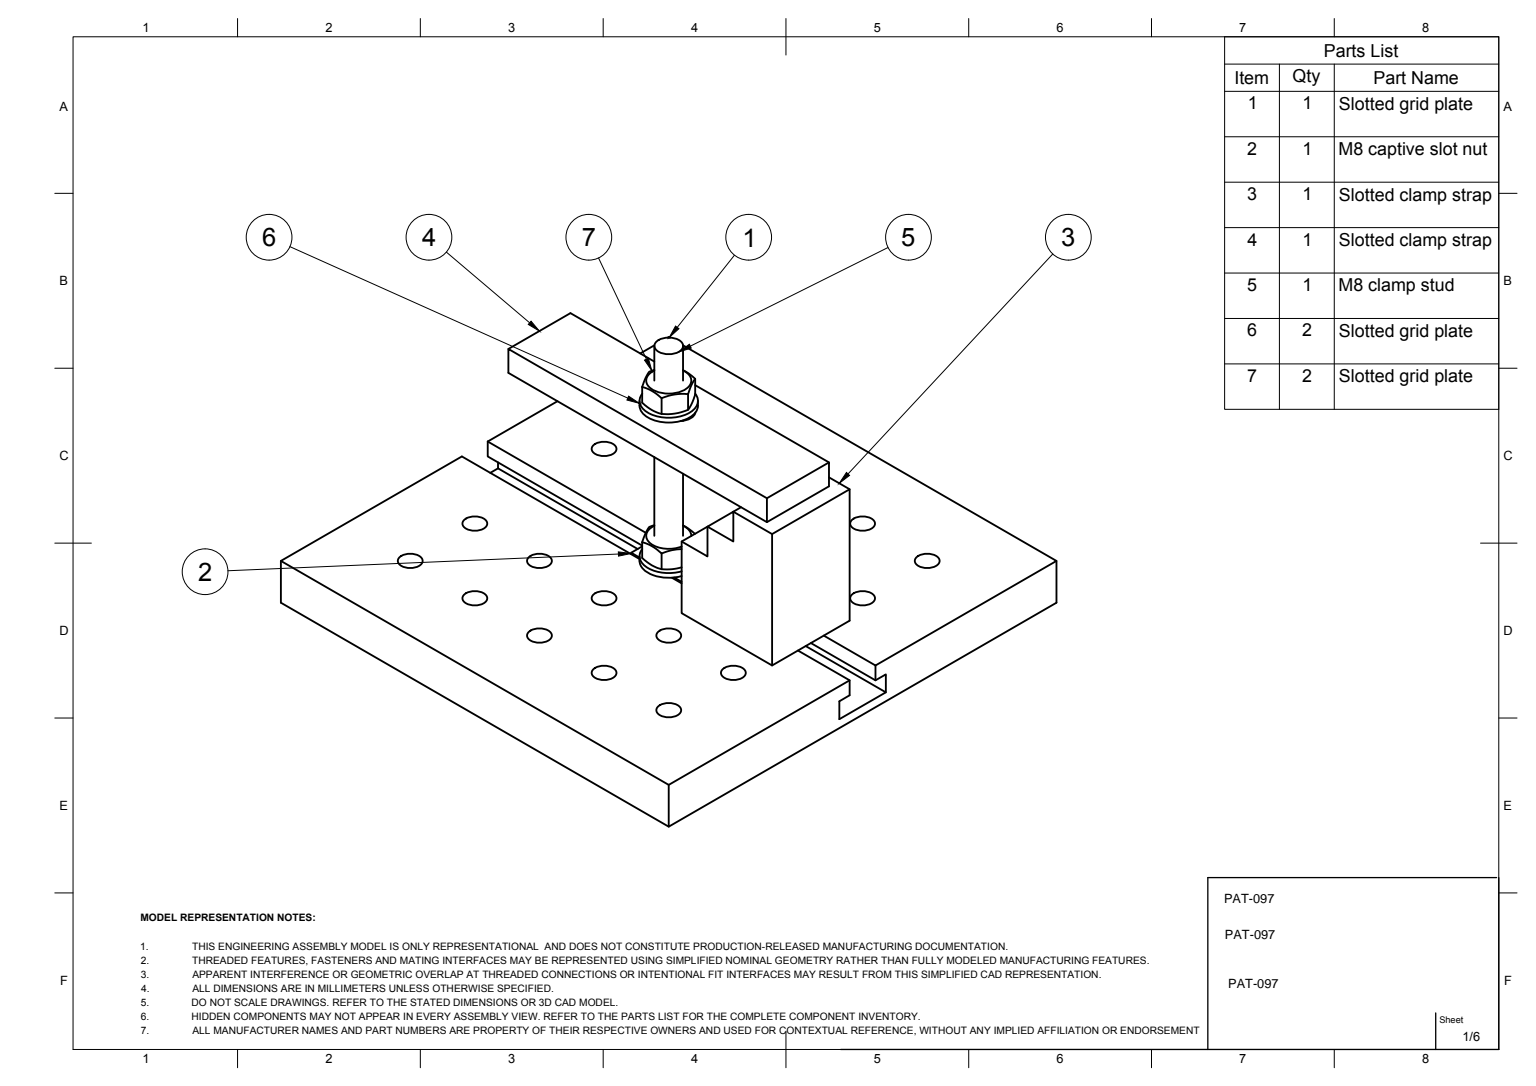
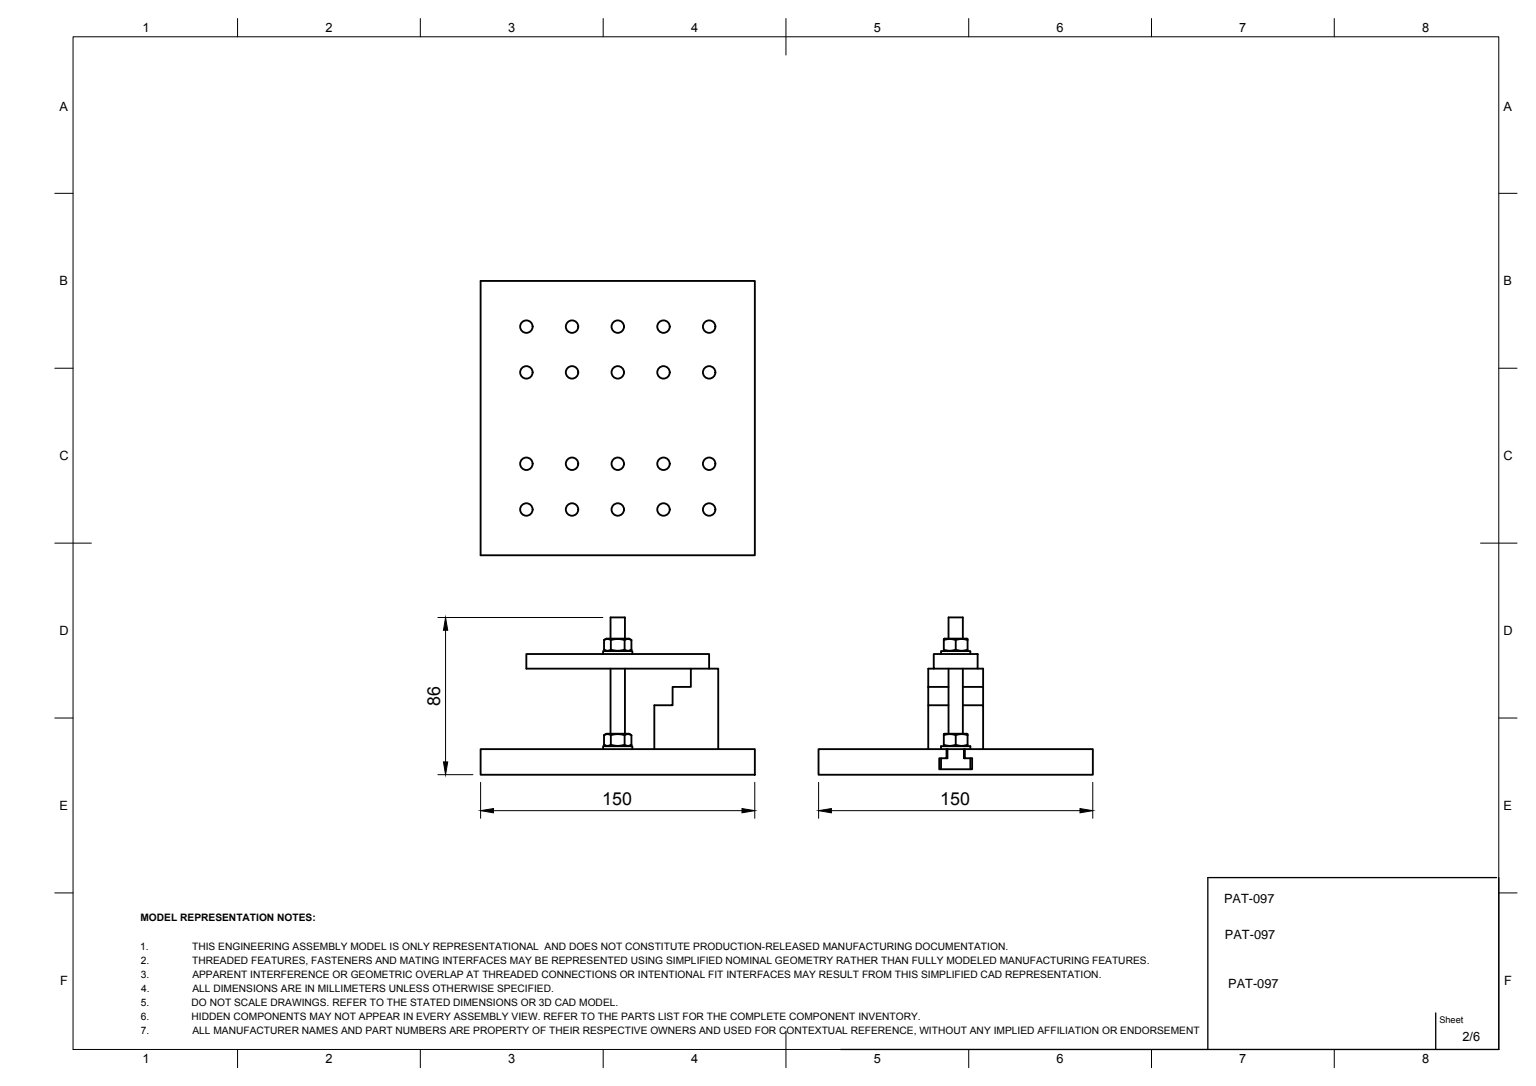
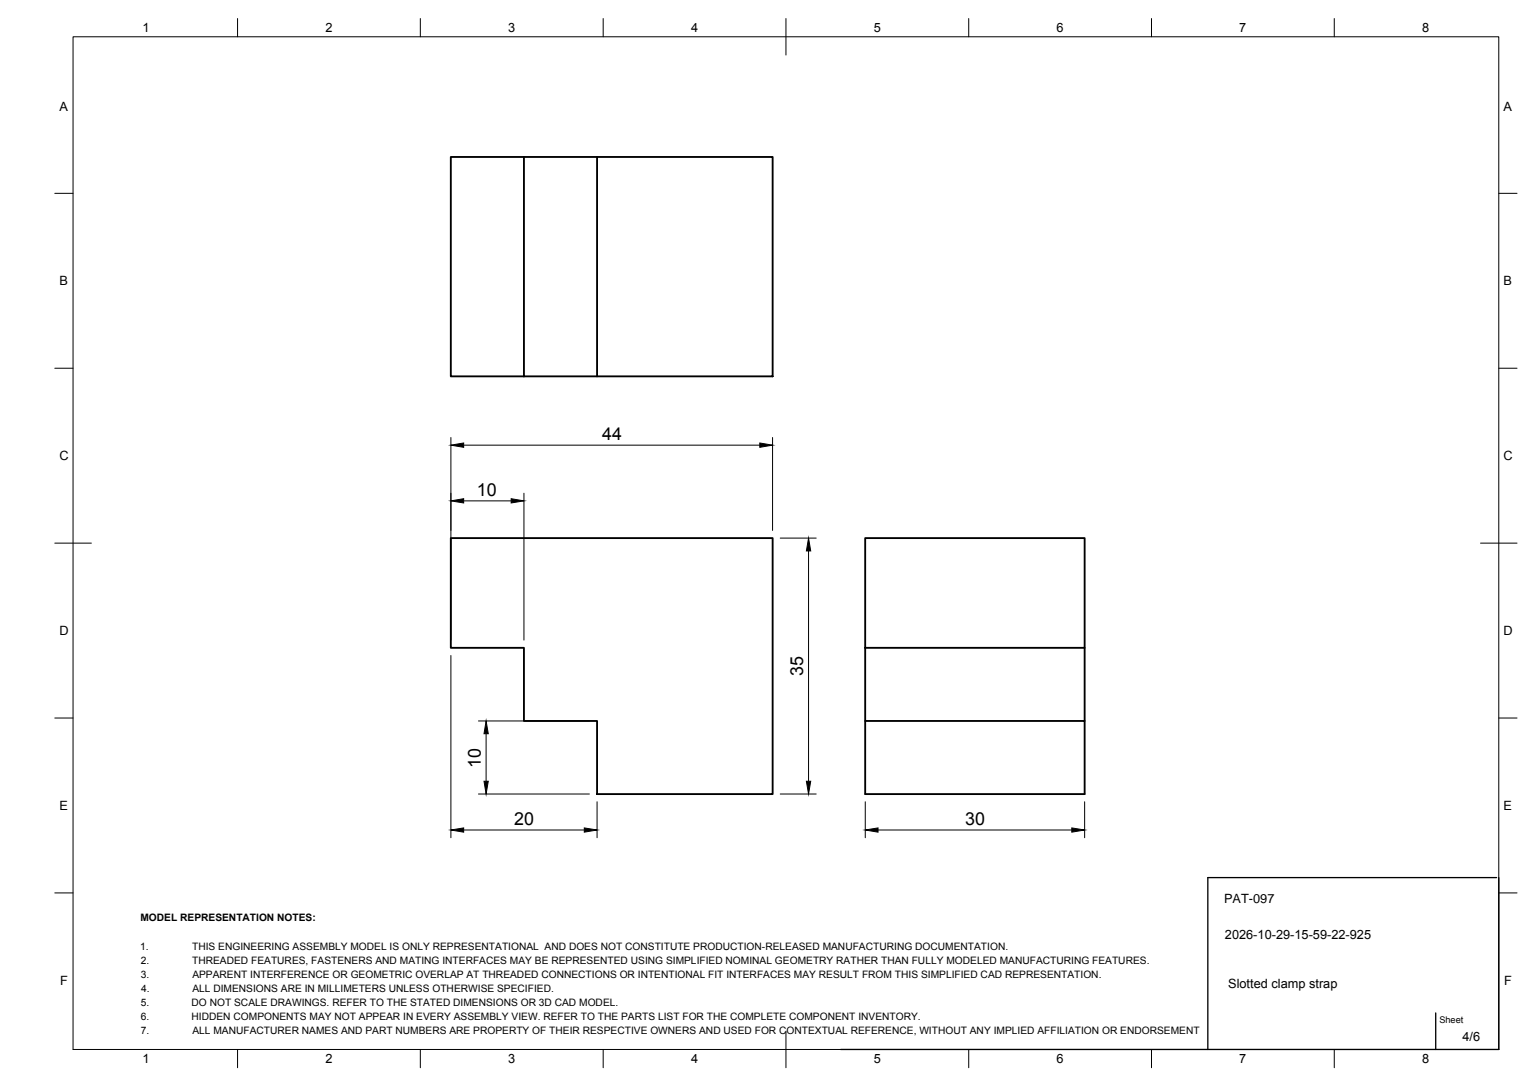
ISO-10303-21;
HEADER;
/* Generated by software containing ST-Developer
 * from STEP Tools, Inc. (www.steptools.com) 
 */

FILE_DESCRIPTION(
/* description */ ('PAT-097'),
/* implementation_level */ '2;1');

FILE_NAME(
/* name */ 'PAT-097',
/* time_stamp */ '2026-10-29T15:59:31-07:00',
/* author */ (''),
/* organization */ (''),
/* preprocessor_version */ 'ST-DEVELOPER v20.2',
/* originating_system */ 'Autodesk Translation Framework v15.17.0.0',
/* authorisation */ '');

FILE_SCHEMA (('AUTOMOTIVE_DESIGN { 1 0 10303 214 3 1 1 }'));
ENDSEC;

DATA;
#10=MECHANICAL_DESIGN_GEOMETRIC_PRESENTATION_REPRESENTATION('',(#75,#76,
#77,#78,#79,#80,#81),#2768);
#11=ITEM_DEFINED_TRANSFORMATION($,$,#1682,#1828);
#12=ITEM_DEFINED_TRANSFORMATION($,$,#1757,#1829);
#13=ITEM_DEFINED_TRANSFORMATION($,$,#1771,#1830);
#14=ITEM_DEFINED_TRANSFORMATION($,$,#1782,#1831);
#15=ITEM_DEFINED_TRANSFORMATION($,$,#1797,#1832);
#16=ITEM_DEFINED_TRANSFORMATION($,$,#1803,#1833);
#17=ITEM_DEFINED_TRANSFORMATION($,$,#1812,#1834);
#18=ITEM_DEFINED_TRANSFORMATION($,$,#1803,#1835);
#19=ITEM_DEFINED_TRANSFORMATION($,$,#1812,#1836);
#20=(
REPRESENTATION_RELATIONSHIP($,$,#2799,#2798)
REPRESENTATION_RELATIONSHIP_WITH_TRANSFORMATION(#11)
SHAPE_REPRESENTATION_RELATIONSHIP()
);
#21=(
REPRESENTATION_RELATIONSHIP($,$,#2800,#2798)
REPRESENTATION_RELATIONSHIP_WITH_TRANSFORMATION(#12)
SHAPE_REPRESENTATION_RELATIONSHIP()
);
#22=(
REPRESENTATION_RELATIONSHIP($,$,#2801,#2798)
REPRESENTATION_RELATIONSHIP_WITH_TRANSFORMATION(#13)
SHAPE_REPRESENTATION_RELATIONSHIP()
);
#23=(
REPRESENTATION_RELATIONSHIP($,$,#2802,#2798)
REPRESENTATION_RELATIONSHIP_WITH_TRANSFORMATION(#14)
SHAPE_REPRESENTATION_RELATIONSHIP()
);
#24=(
REPRESENTATION_RELATIONSHIP($,$,#2803,#2798)
REPRESENTATION_RELATIONSHIP_WITH_TRANSFORMATION(#15)
SHAPE_REPRESENTATION_RELATIONSHIP()
);
#25=(
REPRESENTATION_RELATIONSHIP($,$,#2804,#2798)
REPRESENTATION_RELATIONSHIP_WITH_TRANSFORMATION(#16)
SHAPE_REPRESENTATION_RELATIONSHIP()
);
#26=(
REPRESENTATION_RELATIONSHIP($,$,#2805,#2798)
REPRESENTATION_RELATIONSHIP_WITH_TRANSFORMATION(#17)
SHAPE_REPRESENTATION_RELATIONSHIP()
);
#27=(
REPRESENTATION_RELATIONSHIP($,$,#2804,#2798)
REPRESENTATION_RELATIONSHIP_WITH_TRANSFORMATION(#18)
SHAPE_REPRESENTATION_RELATIONSHIP()
);
#28=(
REPRESENTATION_RELATIONSHIP($,$,#2805,#2798)
REPRESENTATION_RELATIONSHIP_WITH_TRANSFORMATION(#19)
SHAPE_REPRESENTATION_RELATIONSHIP()
);
#29=CONTEXT_DEPENDENT_SHAPE_REPRESENTATION(#20,#2789);
#30=CONTEXT_DEPENDENT_SHAPE_REPRESENTATION(#21,#2790);
#31=CONTEXT_DEPENDENT_SHAPE_REPRESENTATION(#22,#2791);
#32=CONTEXT_DEPENDENT_SHAPE_REPRESENTATION(#23,#2792);
#33=CONTEXT_DEPENDENT_SHAPE_REPRESENTATION(#24,#2793);
#34=CONTEXT_DEPENDENT_SHAPE_REPRESENTATION(#25,#2794);
#35=CONTEXT_DEPENDENT_SHAPE_REPRESENTATION(#26,#2795);
#36=CONTEXT_DEPENDENT_SHAPE_REPRESENTATION(#27,#2796);
#37=CONTEXT_DEPENDENT_SHAPE_REPRESENTATION(#28,#2797);
#38=NEXT_ASSEMBLY_USAGE_OCCURRENCE('Slotted grid plate:1',
'Slotted grid plate:1','Slotted grid plate:1',#2807,#2808,
'Slotted grid plate:1');
#39=NEXT_ASSEMBLY_USAGE_OCCURRENCE('M8 captive slot nut:1',
'M8 captive slot nut:1','M8 captive slot nut:1',#2807,#2809,
'M8 captive slot nut:1');
#40=NEXT_ASSEMBLY_USAGE_OCCURRENCE('Stepped heel block:1',
'Stepped heel block:1','Stepped heel block:1',#2807,#2810,
'Stepped heel block:1');
#41=NEXT_ASSEMBLY_USAGE_OCCURRENCE('Slotted clamp strap:1',
'Slotted clamp strap:1','Slotted clamp strap:1',#2807,#2811,
'Slotted clamp strap:1');
#42=NEXT_ASSEMBLY_USAGE_OCCURRENCE('M8 clamp stud:1','M8 clamp stud:1',
'M8 clamp stud:1',#2807,#2812,'M8 clamp stud:1');
#43=NEXT_ASSEMBLY_USAGE_OCCURRENCE('Flat Washer - M8:1',
'Flat Washer - M8:1','Flat Washer - M8:1',#2807,#2813,
'Flat Washer - M8:1');
#44=NEXT_ASSEMBLY_USAGE_OCCURRENCE('Hex Nut - M8:1','Hex Nut - M8:1',
'Hex Nut - M8:1',#2807,#2814,'Hex Nut - M8:1');
#45=NEXT_ASSEMBLY_USAGE_OCCURRENCE('Flat Washer - M8:2',
'Flat Washer - M8:2','Flat Washer - M8:2',#2807,#2813,
'Flat Washer - M8:2');
#46=NEXT_ASSEMBLY_USAGE_OCCURRENCE('Hex Nut - M8:2','Hex Nut - M8:2',
'Hex Nut - M8:2',#2807,#2814,'Hex Nut - M8:2');
#47=(
BOUNDED_CURVE()
B_SPLINE_CURVE(2,(#2669,#2670,#2671),.UNSPECIFIED.,.F.,.F.)
B_SPLINE_CURVE_WITH_KNOTS((3,3),(0.14973948338295,0.97160236658079),
 .UNSPECIFIED.)
CURVE()
GEOMETRIC_REPRESENTATION_ITEM()
RATIONAL_B_SPLINE_CURVE((1.07140024848292,1.23714644374248,1.07140024848292))
REPRESENTATION_ITEM('')
);
#48=(
BOUNDED_CURVE()
B_SPLINE_CURVE(2,(#2673,#2674,#2675),.UNSPECIFIED.,.F.,.F.)
B_SPLINE_CURVE_WITH_KNOTS((3,3),(0.14973948338295,0.971602366580789),
 .UNSPECIFIED.)
CURVE()
GEOMETRIC_REPRESENTATION_ITEM()
RATIONAL_B_SPLINE_CURVE((1.07140024848292,1.23714644374248,1.07140024848292))
REPRESENTATION_ITEM('')
);
#49=(
BOUNDED_CURVE()
B_SPLINE_CURVE(2,(#2680,#2681,#2682),.UNSPECIFIED.,.F.,.F.)
B_SPLINE_CURVE_WITH_KNOTS((3,3),(0.14973948338295,0.97160236658079),
 .UNSPECIFIED.)
CURVE()
GEOMETRIC_REPRESENTATION_ITEM()
RATIONAL_B_SPLINE_CURVE((1.07140024848292,1.23714644374248,1.07140024848292))
REPRESENTATION_ITEM('')
);
#50=(
BOUNDED_CURVE()
B_SPLINE_CURVE(2,(#2684,#2685,#2686),.UNSPECIFIED.,.F.,.F.)
B_SPLINE_CURVE_WITH_KNOTS((3,3),(0.14973948338295,0.97160236658079),
 .UNSPECIFIED.)
CURVE()
GEOMETRIC_REPRESENTATION_ITEM()
RATIONAL_B_SPLINE_CURVE((1.07140024848292,1.23714644374248,1.07140024848292))
REPRESENTATION_ITEM('')
);
#51=(
BOUNDED_CURVE()
B_SPLINE_CURVE(2,(#2688,#2689,#2690),.UNSPECIFIED.,.F.,.F.)
B_SPLINE_CURVE_WITH_KNOTS((3,3),(0.14973948338295,0.971602366580789),
 .UNSPECIFIED.)
CURVE()
GEOMETRIC_REPRESENTATION_ITEM()
RATIONAL_B_SPLINE_CURVE((1.07140024848292,1.23714644374248,1.07140024848292))
REPRESENTATION_ITEM('')
);
#52=(
BOUNDED_CURVE()
B_SPLINE_CURVE(2,(#2691,#2692,#2693),.UNSPECIFIED.,.F.,.F.)
B_SPLINE_CURVE_WITH_KNOTS((3,3),(0.14973948338295,0.97160236658079),
 .UNSPECIFIED.)
CURVE()
GEOMETRIC_REPRESENTATION_ITEM()
RATIONAL_B_SPLINE_CURVE((1.07140024848292,1.23714644374248,1.07140024848292))
REPRESENTATION_ITEM('')
);
#53=(
BOUNDED_CURVE()
B_SPLINE_CURVE(2,(#2700,#2701,#2702),.UNSPECIFIED.,.F.,.F.)
B_SPLINE_CURVE_WITH_KNOTS((3,3),(0.14973948338295,0.97160236658079),
 .UNSPECIFIED.)
CURVE()
GEOMETRIC_REPRESENTATION_ITEM()
RATIONAL_B_SPLINE_CURVE((1.07140024848292,1.23714644374248,1.07140024848292))
REPRESENTATION_ITEM('')
);
#54=(
BOUNDED_CURVE()
B_SPLINE_CURVE(2,(#2704,#2705,#2706),.UNSPECIFIED.,.F.,.F.)
B_SPLINE_CURVE_WITH_KNOTS((3,3),(0.14973948338295,0.97160236658079),
 .UNSPECIFIED.)
CURVE()
GEOMETRIC_REPRESENTATION_ITEM()
RATIONAL_B_SPLINE_CURVE((1.07140024848292,1.23714644374248,1.07140024848292))
REPRESENTATION_ITEM('')
);
#55=(
BOUNDED_CURVE()
B_SPLINE_CURVE(2,(#2708,#2709,#2710),.UNSPECIFIED.,.F.,.F.)
B_SPLINE_CURVE_WITH_KNOTS((3,3),(0.14973948338295,0.971602366580789),
 .UNSPECIFIED.)
CURVE()
GEOMETRIC_REPRESENTATION_ITEM()
RATIONAL_B_SPLINE_CURVE((1.07140024848292,1.23714644374248,1.07140024848292))
REPRESENTATION_ITEM('')
);
#56=(
BOUNDED_CURVE()
B_SPLINE_CURVE(2,(#2712,#2713,#2714),.UNSPECIFIED.,.F.,.F.)
B_SPLINE_CURVE_WITH_KNOTS((3,3),(0.14973948338295,0.97160236658079),
 .UNSPECIFIED.)
CURVE()
GEOMETRIC_REPRESENTATION_ITEM()
RATIONAL_B_SPLINE_CURVE((1.07140024848292,1.23714644374248,1.07140024848292))
REPRESENTATION_ITEM('')
);
#57=(
BOUNDED_CURVE()
B_SPLINE_CURVE(2,(#2716,#2717,#2718),.UNSPECIFIED.,.F.,.F.)
B_SPLINE_CURVE_WITH_KNOTS((3,3),(0.14973948338295,0.97160236658079),
 .UNSPECIFIED.)
CURVE()
GEOMETRIC_REPRESENTATION_ITEM()
RATIONAL_B_SPLINE_CURVE((1.07140024848292,1.23714644374248,1.07140024848292))
REPRESENTATION_ITEM('')
);
#58=(
BOUNDED_CURVE()
B_SPLINE_CURVE(2,(#2719,#2720,#2721),.UNSPECIFIED.,.F.,.F.)
B_SPLINE_CURVE_WITH_KNOTS((3,3),(0.14973948338295,0.971602366580789),
 .UNSPECIFIED.)
CURVE()
GEOMETRIC_REPRESENTATION_ITEM()
RATIONAL_B_SPLINE_CURVE((1.07140024848292,1.23714644374248,1.07140024848292))
REPRESENTATION_ITEM('')
);
#59=CONICAL_SURFACE('',#1813,0.734027674973257,1.0471975511966);
#60=CONICAL_SURFACE('',#1815,0.734027674973257,1.0471975511966);
#61=SHAPE_REPRESENTATION_RELATIONSHIP('SRR','None',#2799,#68);
#62=SHAPE_REPRESENTATION_RELATIONSHIP('SRR','None',#2800,#69);
#63=SHAPE_REPRESENTATION_RELATIONSHIP('SRR','None',#2801,#70);
#64=SHAPE_REPRESENTATION_RELATIONSHIP('SRR','None',#2802,#71);
#65=SHAPE_REPRESENTATION_RELATIONSHIP('SRR','None',#2803,#72);
#66=SHAPE_REPRESENTATION_RELATIONSHIP('SRR','None',#2804,#73);
#67=SHAPE_REPRESENTATION_RELATIONSHIP('SRR','None',#2805,#74);
#68=ADVANCED_BREP_SHAPE_REPRESENTATION('',(#82),#2761);
#69=ADVANCED_BREP_SHAPE_REPRESENTATION('',(#83),#2762);
#70=ADVANCED_BREP_SHAPE_REPRESENTATION('',(#84),#2763);
#71=ADVANCED_BREP_SHAPE_REPRESENTATION('',(#85),#2764);
#72=ADVANCED_BREP_SHAPE_REPRESENTATION('',(#86),#2765);
#73=ADVANCED_BREP_SHAPE_REPRESENTATION('',(#87),#2766);
#74=ADVANCED_BREP_SHAPE_REPRESENTATION('',(#88),#2767);
#75=STYLED_ITEM('',(#2925),#82);
#76=STYLED_ITEM('',(#2918),#83);
#77=STYLED_ITEM('',(#2890),#84);
#78=STYLED_ITEM('',(#2925),#85);
#79=STYLED_ITEM('',(#2918),#86);
#80=STYLED_ITEM('',(#2918),#87);
#81=STYLED_ITEM('',(#2918),#88);
#82=MANIFOLD_SOLID_BREP('Body1',#1596);
#83=MANIFOLD_SOLID_BREP('Body1',#1597);
#84=MANIFOLD_SOLID_BREP('Body1',#1598);
#85=MANIFOLD_SOLID_BREP('Body1',#1599);
#86=MANIFOLD_SOLID_BREP('Body1',#1600);
#87=MANIFOLD_SOLID_BREP('Body1',#1601);
#88=MANIFOLD_SOLID_BREP('Body1',#1602);
#89=CYLINDRICAL_SURFACE('',#1713,0.34);
#90=CYLINDRICAL_SURFACE('',#1715,0.34);
#91=CYLINDRICAL_SURFACE('',#1717,0.34);
#92=CYLINDRICAL_SURFACE('',#1719,0.34);
#93=CYLINDRICAL_SURFACE('',#1721,0.34);
#94=CYLINDRICAL_SURFACE('',#1723,0.34);
#95=CYLINDRICAL_SURFACE('',#1725,0.34);
#96=CYLINDRICAL_SURFACE('',#1727,0.34);
#97=CYLINDRICAL_SURFACE('',#1729,0.34);
#98=CYLINDRICAL_SURFACE('',#1731,0.34);
#99=CYLINDRICAL_SURFACE('',#1733,0.34);
#100=CYLINDRICAL_SURFACE('',#1735,0.34);
#101=CYLINDRICAL_SURFACE('',#1737,0.34);
#102=CYLINDRICAL_SURFACE('',#1739,0.34);
#103=CYLINDRICAL_SURFACE('',#1741,0.34);
#104=CYLINDRICAL_SURFACE('',#1743,0.34);
#105=CYLINDRICAL_SURFACE('',#1745,0.34);
#106=CYLINDRICAL_SURFACE('',#1747,0.34);
#107=CYLINDRICAL_SURFACE('',#1749,0.34);
#108=CYLINDRICAL_SURFACE('',#1751,0.34);
#109=CYLINDRICAL_SURFACE('',#1758,0.34);
#110=CYLINDRICAL_SURFACE('',#1788,0.45);
#111=CYLINDRICAL_SURFACE('',#1790,0.45);
#112=CYLINDRICAL_SURFACE('',#1798,0.3933);
#113=CYLINDRICAL_SURFACE('',#1804,0.42);
#114=CYLINDRICAL_SURFACE('',#1807,0.8);
#115=CYLINDRICAL_SURFACE('',#1820,0.338975);
#116=FACE_BOUND('',#312,.T.);
#117=FACE_BOUND('',#313,.T.);
#118=FACE_BOUND('',#314,.T.);
#119=FACE_BOUND('',#315,.T.);
#120=FACE_BOUND('',#316,.T.);
#121=FACE_BOUND('',#317,.T.);
#122=FACE_BOUND('',#318,.T.);
#123=FACE_BOUND('',#319,.T.);
#124=FACE_BOUND('',#320,.T.);
#125=FACE_BOUND('',#321,.T.);
#126=FACE_BOUND('',#323,.T.);
#127=FACE_BOUND('',#324,.T.);
#128=FACE_BOUND('',#325,.T.);
#129=FACE_BOUND('',#326,.T.);
#130=FACE_BOUND('',#327,.T.);
#131=FACE_BOUND('',#328,.T.);
#132=FACE_BOUND('',#329,.T.);
#133=FACE_BOUND('',#330,.T.);
#134=FACE_BOUND('',#331,.T.);
#135=FACE_BOUND('',#332,.T.);
#136=FACE_BOUND('',#357,.T.);
#137=FACE_BOUND('',#358,.T.);
#138=FACE_BOUND('',#359,.T.);
#139=FACE_BOUND('',#360,.T.);
#140=FACE_BOUND('',#361,.T.);
#141=FACE_BOUND('',#362,.T.);
#142=FACE_BOUND('',#363,.T.);
#143=FACE_BOUND('',#364,.T.);
#144=FACE_BOUND('',#365,.T.);
#145=FACE_BOUND('',#366,.T.);
#146=FACE_BOUND('',#367,.T.);
#147=FACE_BOUND('',#368,.T.);
#148=FACE_BOUND('',#369,.T.);
#149=FACE_BOUND('',#370,.T.);
#150=FACE_BOUND('',#371,.T.);
#151=FACE_BOUND('',#372,.T.);
#152=FACE_BOUND('',#373,.T.);
#153=FACE_BOUND('',#374,.T.);
#154=FACE_BOUND('',#375,.T.);
#155=FACE_BOUND('',#376,.T.);
#156=FACE_BOUND('',#381,.T.);
#157=FACE_BOUND('',#389,.T.);
#158=FACE_BOUND('',#403,.T.);
#159=FACE_BOUND('',#411,.T.);
#160=FACE_BOUND('',#418,.T.);
#161=FACE_BOUND('',#420,.T.);
#162=FACE_BOUND('',#431,.T.);
#163=FACE_BOUND('',#433,.T.);
#164=CIRCLE('',#1692,0.34);
#165=CIRCLE('',#1693,0.34);
#166=CIRCLE('',#1694,0.34);
#167=CIRCLE('',#1695,0.34);
#168=CIRCLE('',#1696,0.34);
#169=CIRCLE('',#1697,0.34);
#170=CIRCLE('',#1698,0.34);
#171=CIRCLE('',#1699,0.34);
#172=CIRCLE('',#1700,0.34);
#173=CIRCLE('',#1701,0.34);
#174=CIRCLE('',#1703,0.34);
#175=CIRCLE('',#1704,0.34);
#176=CIRCLE('',#1705,0.34);
#177=CIRCLE('',#1706,0.34);
#178=CIRCLE('',#1707,0.34);
#179=CIRCLE('',#1708,0.34);
#180=CIRCLE('',#1709,0.34);
#181=CIRCLE('',#1710,0.34);
#182=CIRCLE('',#1711,0.34);
#183=CIRCLE('',#1712,0.34);
#184=CIRCLE('',#1714,0.34);
#185=CIRCLE('',#1716,0.34);
#186=CIRCLE('',#1718,0.34);
#187=CIRCLE('',#1720,0.34);
#188=CIRCLE('',#1722,0.34);
#189=CIRCLE('',#1724,0.34);
#190=CIRCLE('',#1726,0.34);
#191=CIRCLE('',#1728,0.34);
#192=CIRCLE('',#1730,0.34);
#193=CIRCLE('',#1732,0.34);
#194=CIRCLE('',#1734,0.34);
#195=CIRCLE('',#1736,0.34);
#196=CIRCLE('',#1738,0.34);
#197=CIRCLE('',#1740,0.34);
#198=CIRCLE('',#1742,0.34);
#199=CIRCLE('',#1744,0.34);
#200=CIRCLE('',#1746,0.34);
#201=CIRCLE('',#1748,0.34);
#202=CIRCLE('',#1750,0.34);
#203=CIRCLE('',#1752,0.34);
#204=CIRCLE('',#1759,0.34);
#205=CIRCLE('',#1760,0.34);
#206=CIRCLE('',#1786,0.45);
#207=CIRCLE('',#1787,0.45);
#208=CIRCLE('',#1789,0.45);
#209=CIRCLE('',#1791,0.45);
#210=CIRCLE('',#1799,0.3933);
#211=CIRCLE('',#1800,0.3933);
#212=CIRCLE('',#1805,0.42);
#213=CIRCLE('',#1806,0.42);
#214=CIRCLE('',#1808,0.8);
#215=CIRCLE('',#1809,0.8);
#216=CIRCLE('',#1814,0.6175);
#217=CIRCLE('',#1816,0.6175);
#218=CIRCLE('',#1821,0.338975);
#219=CIRCLE('',#1822,0.338975);
#220=FACE_OUTER_BOUND('',#303,.T.);
#221=FACE_OUTER_BOUND('',#304,.T.);
#222=FACE_OUTER_BOUND('',#305,.T.);
#223=FACE_OUTER_BOUND('',#306,.T.);
#224=FACE_OUTER_BOUND('',#307,.T.);
#225=FACE_OUTER_BOUND('',#308,.T.);
#226=FACE_OUTER_BOUND('',#309,.T.);
#227=FACE_OUTER_BOUND('',#310,.T.);
#228=FACE_OUTER_BOUND('',#311,.T.);
#229=FACE_OUTER_BOUND('',#322,.T.);
#230=FACE_OUTER_BOUND('',#333,.T.);
#231=FACE_OUTER_BOUND('',#334,.T.);
#232=FACE_OUTER_BOUND('',#335,.T.);
#233=FACE_OUTER_BOUND('',#336,.T.);
#234=FACE_OUTER_BOUND('',#337,.T.);
#235=FACE_OUTER_BOUND('',#338,.T.);
#236=FACE_OUTER_BOUND('',#339,.T.);
#237=FACE_OUTER_BOUND('',#340,.T.);
#238=FACE_OUTER_BOUND('',#341,.T.);
#239=FACE_OUTER_BOUND('',#342,.T.);
#240=FACE_OUTER_BOUND('',#343,.T.);
#241=FACE_OUTER_BOUND('',#344,.T.);
#242=FACE_OUTER_BOUND('',#345,.T.);
#243=FACE_OUTER_BOUND('',#346,.T.);
#244=FACE_OUTER_BOUND('',#347,.T.);
#245=FACE_OUTER_BOUND('',#348,.T.);
#246=FACE_OUTER_BOUND('',#349,.T.);
#247=FACE_OUTER_BOUND('',#350,.T.);
#248=FACE_OUTER_BOUND('',#351,.T.);
#249=FACE_OUTER_BOUND('',#352,.T.);
#250=FACE_OUTER_BOUND('',#353,.T.);
#251=FACE_OUTER_BOUND('',#354,.T.);
#252=FACE_OUTER_BOUND('',#355,.T.);
#253=FACE_OUTER_BOUND('',#356,.T.);
#254=FACE_OUTER_BOUND('',#377,.T.);
#255=FACE_OUTER_BOUND('',#378,.T.);
#256=FACE_OUTER_BOUND('',#379,.T.);
#257=FACE_OUTER_BOUND('',#380,.T.);
#258=FACE_OUTER_BOUND('',#382,.T.);
#259=FACE_OUTER_BOUND('',#383,.T.);
#260=FACE_OUTER_BOUND('',#384,.T.);
#261=FACE_OUTER_BOUND('',#385,.T.);
#262=FACE_OUTER_BOUND('',#386,.T.);
#263=FACE_OUTER_BOUND('',#387,.T.);
#264=FACE_OUTER_BOUND('',#388,.T.);
#265=FACE_OUTER_BOUND('',#390,.T.);
#266=FACE_OUTER_BOUND('',#391,.T.);
#267=FACE_OUTER_BOUND('',#392,.T.);
#268=FACE_OUTER_BOUND('',#393,.T.);
#269=FACE_OUTER_BOUND('',#394,.T.);
#270=FACE_OUTER_BOUND('',#395,.T.);
#271=FACE_OUTER_BOUND('',#396,.T.);
#272=FACE_OUTER_BOUND('',#397,.T.);
#273=FACE_OUTER_BOUND('',#398,.T.);
#274=FACE_OUTER_BOUND('',#399,.T.);
#275=FACE_OUTER_BOUND('',#400,.T.);
#276=FACE_OUTER_BOUND('',#401,.T.);
#277=FACE_OUTER_BOUND('',#402,.T.);
#278=FACE_OUTER_BOUND('',#404,.T.);
#279=FACE_OUTER_BOUND('',#405,.T.);
#280=FACE_OUTER_BOUND('',#406,.T.);
#281=FACE_OUTER_BOUND('',#407,.T.);
#282=FACE_OUTER_BOUND('',#408,.T.);
#283=FACE_OUTER_BOUND('',#409,.T.);
#284=FACE_OUTER_BOUND('',#410,.T.);
#285=FACE_OUTER_BOUND('',#412,.T.);
#286=FACE_OUTER_BOUND('',#413,.T.);
#287=FACE_OUTER_BOUND('',#414,.T.);
#288=FACE_OUTER_BOUND('',#415,.T.);
#289=FACE_OUTER_BOUND('',#416,.T.);
#290=FACE_OUTER_BOUND('',#417,.T.);
#291=FACE_OUTER_BOUND('',#419,.T.);
#292=FACE_OUTER_BOUND('',#421,.T.);
#293=FACE_OUTER_BOUND('',#422,.T.);
#294=FACE_OUTER_BOUND('',#423,.T.);
#295=FACE_OUTER_BOUND('',#424,.T.);
#296=FACE_OUTER_BOUND('',#425,.T.);
#297=FACE_OUTER_BOUND('',#426,.T.);
#298=FACE_OUTER_BOUND('',#427,.T.);
#299=FACE_OUTER_BOUND('',#428,.T.);
#300=FACE_OUTER_BOUND('',#429,.T.);
#301=FACE_OUTER_BOUND('',#430,.T.);
#302=FACE_OUTER_BOUND('',#432,.T.);
#303=EDGE_LOOP('',(#1049,#1050,#1051,#1052));
#304=EDGE_LOOP('',(#1053,#1054,#1055,#1056));
#305=EDGE_LOOP('',(#1057,#1058,#1059,#1060));
#306=EDGE_LOOP('',(#1061,#1062,#1063,#1064));
#307=EDGE_LOOP('',(#1065,#1066,#1067,#1068));
#308=EDGE_LOOP('',(#1069,#1070,#1071,#1072));
#309=EDGE_LOOP('',(#1073,#1074,#1075,#1076));
#310=EDGE_LOOP('',(#1077,#1078,#1079,#1080,#1081,#1082,#1083,#1084,#1085,
#1086,#1087,#1088));
#311=EDGE_LOOP('',(#1089,#1090,#1091,#1092));
#312=EDGE_LOOP('',(#1093));
#313=EDGE_LOOP('',(#1094));
#314=EDGE_LOOP('',(#1095));
#315=EDGE_LOOP('',(#1096));
#316=EDGE_LOOP('',(#1097));
#317=EDGE_LOOP('',(#1098));
#318=EDGE_LOOP('',(#1099));
#319=EDGE_LOOP('',(#1100));
#320=EDGE_LOOP('',(#1101));
#321=EDGE_LOOP('',(#1102));
#322=EDGE_LOOP('',(#1103,#1104,#1105,#1106));
#323=EDGE_LOOP('',(#1107));
#324=EDGE_LOOP('',(#1108));
#325=EDGE_LOOP('',(#1109));
#326=EDGE_LOOP('',(#1110));
#327=EDGE_LOOP('',(#1111));
#328=EDGE_LOOP('',(#1112));
#329=EDGE_LOOP('',(#1113));
#330=EDGE_LOOP('',(#1114));
#331=EDGE_LOOP('',(#1115));
#332=EDGE_LOOP('',(#1116));
#333=EDGE_LOOP('',(#1117,#1118,#1119,#1120));
#334=EDGE_LOOP('',(#1121,#1122,#1123,#1124));
#335=EDGE_LOOP('',(#1125,#1126,#1127,#1128));
#336=EDGE_LOOP('',(#1129,#1130,#1131,#1132));
#337=EDGE_LOOP('',(#1133,#1134,#1135,#1136));
#338=EDGE_LOOP('',(#1137,#1138,#1139,#1140));
#339=EDGE_LOOP('',(#1141,#1142,#1143,#1144));
#340=EDGE_LOOP('',(#1145,#1146,#1147,#1148));
#341=EDGE_LOOP('',(#1149,#1150,#1151,#1152));
#342=EDGE_LOOP('',(#1153,#1154,#1155,#1156));
#343=EDGE_LOOP('',(#1157,#1158,#1159,#1160));
#344=EDGE_LOOP('',(#1161,#1162,#1163,#1164));
#345=EDGE_LOOP('',(#1165,#1166,#1167,#1168));
#346=EDGE_LOOP('',(#1169,#1170,#1171,#1172));
#347=EDGE_LOOP('',(#1173,#1174,#1175,#1176));
#348=EDGE_LOOP('',(#1177,#1178,#1179,#1180));
#349=EDGE_LOOP('',(#1181,#1182,#1183,#1184));
#350=EDGE_LOOP('',(#1185,#1186,#1187,#1188));
#351=EDGE_LOOP('',(#1189,#1190,#1191,#1192));
#352=EDGE_LOOP('',(#1193,#1194,#1195,#1196));
#353=EDGE_LOOP('',(#1197,#1198,#1199,#1200));
#354=EDGE_LOOP('',(#1201,#1202,#1203,#1204,#1205,#1206,#1207,#1208,#1209,
#1210,#1211,#1212));
#355=EDGE_LOOP('',(#1213,#1214,#1215,#1216));
#356=EDGE_LOOP('',(#1217,#1218,#1219,#1220));
#357=EDGE_LOOP('',(#1221));
#358=EDGE_LOOP('',(#1222));
#359=EDGE_LOOP('',(#1223));
#360=EDGE_LOOP('',(#1224));
#361=EDGE_LOOP('',(#1225));
#362=EDGE_LOOP('',(#1226));
#363=EDGE_LOOP('',(#1227));
#364=EDGE_LOOP('',(#1228));
#365=EDGE_LOOP('',(#1229));
#366=EDGE_LOOP('',(#1230));
#367=EDGE_LOOP('',(#1231));
#368=EDGE_LOOP('',(#1232));
#369=EDGE_LOOP('',(#1233));
#370=EDGE_LOOP('',(#1234));
#371=EDGE_LOOP('',(#1235));
#372=EDGE_LOOP('',(#1236));
#373=EDGE_LOOP('',(#1237));
#374=EDGE_LOOP('',(#1238));
#375=EDGE_LOOP('',(#1239));
#376=EDGE_LOOP('',(#1240));
#377=EDGE_LOOP('',(#1241,#1242,#1243,#1244));
#378=EDGE_LOOP('',(#1245,#1246,#1247,#1248));
#379=EDGE_LOOP('',(#1249,#1250,#1251,#1252));
#380=EDGE_LOOP('',(#1253,#1254,#1255,#1256));
#381=EDGE_LOOP('',(#1257));
#382=EDGE_LOOP('',(#1258,#1259,#1260,#1261));
#383=EDGE_LOOP('',(#1262,#1263,#1264,#1265));
#384=EDGE_LOOP('',(#1266,#1267,#1268,#1269));
#385=EDGE_LOOP('',(#1270,#1271,#1272,#1273,#1274,#1275,#1276,#1277));
#386=EDGE_LOOP('',(#1278,#1279,#1280,#1281));
#387=EDGE_LOOP('',(#1282,#1283,#1284,#1285,#1286,#1287,#1288,#1289));
#388=EDGE_LOOP('',(#1290,#1291,#1292,#1293));
#389=EDGE_LOOP('',(#1294));
#390=EDGE_LOOP('',(#1295,#1296,#1297,#1298));
#391=EDGE_LOOP('',(#1299,#1300,#1301,#1302));
#392=EDGE_LOOP('',(#1303,#1304,#1305,#1306));
#393=EDGE_LOOP('',(#1307,#1308,#1309,#1310));
#394=EDGE_LOOP('',(#1311,#1312,#1313,#1314));
#395=EDGE_LOOP('',(#1315,#1316,#1317,#1318));
#396=EDGE_LOOP('',(#1319,#1320,#1321,#1322));
#397=EDGE_LOOP('',(#1323,#1324,#1325,#1326));
#398=EDGE_LOOP('',(#1327,#1328,#1329,#1330,#1331,#1332,#1333,#1334));
#399=EDGE_LOOP('',(#1335,#1336,#1337,#1338,#1339,#1340,#1341,#1342));
#400=EDGE_LOOP('',(#1343,#1344,#1345,#1346));
#401=EDGE_LOOP('',(#1347,#1348,#1349,#1350));
#402=EDGE_LOOP('',(#1351,#1352,#1353,#1354));
#403=EDGE_LOOP('',(#1355,#1356,#1357,#1358));
#404=EDGE_LOOP('',(#1359,#1360,#1361,#1362));
#405=EDGE_LOOP('',(#1363,#1364,#1365,#1366));
#406=EDGE_LOOP('',(#1367,#1368,#1369,#1370));
#407=EDGE_LOOP('',(#1371,#1372,#1373,#1374));
#408=EDGE_LOOP('',(#1375,#1376,#1377,#1378));
#409=EDGE_LOOP('',(#1379,#1380,#1381,#1382));
#410=EDGE_LOOP('',(#1383,#1384,#1385,#1386));
#411=EDGE_LOOP('',(#1387,#1388,#1389,#1390));
#412=EDGE_LOOP('',(#1391,#1392,#1393,#1394));
#413=EDGE_LOOP('',(#1395));
#414=EDGE_LOOP('',(#1396));
#415=EDGE_LOOP('',(#1397,#1398,#1399,#1400));
#416=EDGE_LOOP('',(#1401,#1402,#1403,#1404));
#417=EDGE_LOOP('',(#1405));
#418=EDGE_LOOP('',(#1406));
#419=EDGE_LOOP('',(#1407));
#420=EDGE_LOOP('',(#1408));
#421=EDGE_LOOP('',(#1409,#1410,#1411,#1412,#1413,#1414,#1415,#1416,#1417));
#422=EDGE_LOOP('',(#1418,#1419,#1420,#1421,#1422,#1423,#1424,#1425,#1426));
#423=EDGE_LOOP('',(#1427,#1428,#1429,#1430));
#424=EDGE_LOOP('',(#1431,#1432,#1433,#1434));
#425=EDGE_LOOP('',(#1435,#1436,#1437,#1438));
#426=EDGE_LOOP('',(#1439,#1440,#1441,#1442));
#427=EDGE_LOOP('',(#1443,#1444,#1445,#1446));
#428=EDGE_LOOP('',(#1447,#1448,#1449,#1450));
#429=EDGE_LOOP('',(#1451,#1452,#1453,#1454));
#430=EDGE_LOOP('',(#1455));
#431=EDGE_LOOP('',(#1456));
#432=EDGE_LOOP('',(#1457));
#433=EDGE_LOOP('',(#1458));
#434=LINE('',#2291,#571);
#435=LINE('',#2293,#572);
#436=LINE('',#2295,#573);
#437=LINE('',#2296,#574);
#438=LINE('',#2299,#575);
#439=LINE('',#2301,#576);
#440=LINE('',#2302,#577);
#441=LINE('',#2306,#578);
#442=LINE('',#2308,#579);
#443=LINE('',#2310,#580);
#444=LINE('',#2311,#581);
#445=LINE('',#2314,#582);
#446=LINE('',#2316,#583);
#447=LINE('',#2317,#584);
#448=LINE('',#2320,#585);
#449=LINE('',#2322,#586);
#450=LINE('',#2323,#587);
#451=LINE('',#2326,#588);
#452=LINE('',#2328,#589);
#453=LINE('',#2329,#590);
#454=LINE('',#2331,#591);
#455=LINE('',#2332,#592);
#456=LINE('',#2335,#593);
#457=LINE('',#2337,#594);
#458=LINE('',#2339,#595);
#459=LINE('',#2341,#596);
#460=LINE('',#2342,#597);
#461=LINE('',#2345,#598);
#462=LINE('',#2346,#599);
#463=LINE('',#2369,#600);
#464=LINE('',#2370,#601);
#465=LINE('',#2394,#602);
#466=LINE('',#2398,#603);
#467=LINE('',#2402,#604);
#468=LINE('',#2406,#605);
#469=LINE('',#2410,#606);
#470=LINE('',#2414,#607);
#471=LINE('',#2418,#608);
#472=LINE('',#2422,#609);
#473=LINE('',#2426,#610);
#474=LINE('',#2430,#611);
#475=LINE('',#2434,#612);
#476=LINE('',#2438,#613);
#477=LINE('',#2442,#614);
#478=LINE('',#2446,#615);
#479=LINE('',#2450,#616);
#480=LINE('',#2454,#617);
#481=LINE('',#2458,#618);
#482=LINE('',#2462,#619);
#483=LINE('',#2466,#620);
#484=LINE('',#2470,#621);
#485=LINE('',#2473,#622);
#486=LINE('',#2474,#623);
#487=LINE('',#2477,#624);
#488=LINE('',#2478,#625);
#489=LINE('',#2480,#626);
#490=LINE('',#2487,#627);
#491=LINE('',#2492,#628);
#492=LINE('',#2494,#629);
#493=LINE('',#2496,#630);
#494=LINE('',#2497,#631);
#495=LINE('',#2501,#632);
#496=LINE('',#2503,#633);
#497=LINE('',#2505,#634);
#498=LINE('',#2506,#635);
#499=LINE('',#2508,#636);
#500=LINE('',#2509,#637);
#501=LINE('',#2512,#638);
#502=LINE('',#2514,#639);
#503=LINE('',#2515,#640);
#504=LINE('',#2518,#641);
#505=LINE('',#2520,#642);
#506=LINE('',#2521,#643);
#507=LINE('',#2525,#644);
#508=LINE('',#2526,#645);
#509=LINE('',#2527,#646);
#510=LINE('',#2530,#647);
#511=LINE('',#2531,#648);
#512=LINE('',#2534,#649);
#513=LINE('',#2535,#650);
#514=LINE('',#2537,#651);
#515=LINE('',#2543,#652);
#516=LINE('',#2545,#653);
#517=LINE('',#2547,#654);
#518=LINE('',#2548,#655);
#519=LINE('',#2551,#656);
#520=LINE('',#2553,#657);
#521=LINE('',#2554,#658);
#522=LINE('',#2557,#659);
#523=LINE('',#2559,#660);
#524=LINE('',#2560,#661);
#525=LINE('',#2563,#662);
#526=LINE('',#2565,#663);
#527=LINE('',#2566,#664);
#528=LINE('',#2569,#665);
#529=LINE('',#2571,#666);
#530=LINE('',#2572,#667);
#531=LINE('',#2575,#668);
#532=LINE('',#2577,#669);
#533=LINE('',#2578,#670);
#534=LINE('',#2581,#671);
#535=LINE('',#2583,#672);
#536=LINE('',#2584,#673);
#537=LINE('',#2586,#674);
#538=LINE('',#2587,#675);
#539=LINE('',#2594,#676);
#540=LINE('',#2596,#677);
#541=LINE('',#2598,#678);
#542=LINE('',#2599,#679);
#543=LINE('',#2603,#680);
#544=LINE('',#2605,#681);
#545=LINE('',#2607,#682);
#546=LINE('',#2608,#683);
#547=LINE('',#2612,#684);
#548=LINE('',#2614,#685);
#549=LINE('',#2616,#686);
#550=LINE('',#2617,#687);
#551=LINE('',#2626,#688);
#552=LINE('',#2628,#689);
#553=LINE('',#2629,#690);
#554=LINE('',#2632,#691);
#555=LINE('',#2633,#692);
#556=LINE('',#2636,#693);
#557=LINE('',#2637,#694);
#558=LINE('',#2639,#695);
#559=LINE('',#2646,#696);
#560=LINE('',#2655,#697);
#561=LINE('',#2661,#698);
#562=LINE('',#2677,#699);
#563=LINE('',#2698,#700);
#564=LINE('',#2723,#701);
#565=LINE('',#2724,#702);
#566=LINE('',#2726,#703);
#567=LINE('',#2728,#704);
#568=LINE('',#2733,#705);
#569=LINE('',#2736,#706);
#570=LINE('',#2738,#707);
#571=VECTOR('',#1843,1.);
#572=VECTOR('',#1844,1.);
#573=VECTOR('',#1845,1.);
#574=VECTOR('',#1846,1.);
#575=VECTOR('',#1849,1.);
#576=VECTOR('',#1850,1.);
#577=VECTOR('',#1851,1.);
#578=VECTOR('',#1854,1.);
#579=VECTOR('',#1855,1.);
#580=VECTOR('',#1856,1.);
#581=VECTOR('',#1857,1.);
#582=VECTOR('',#1860,1.);
#583=VECTOR('',#1861,1.);
#584=VECTOR('',#1862,1.);
#585=VECTOR('',#1865,1.);
#586=VECTOR('',#1866,1.);
#587=VECTOR('',#1867,1.);
#588=VECTOR('',#1870,1.);
#589=VECTOR('',#1871,1.);
#590=VECTOR('',#1872,1.);
#591=VECTOR('',#1875,1.);
#592=VECTOR('',#1876,1.);
#593=VECTOR('',#1879,1.);
#594=VECTOR('',#1880,1.);
#595=VECTOR('',#1881,1.);
#596=VECTOR('',#1882,1.);
#597=VECTOR('',#1883,1.);
#598=VECTOR('',#1886,1.);
#599=VECTOR('',#1887,1.);
#600=VECTOR('',#1910,1.);
#601=VECTOR('',#1911,1.);
#602=VECTOR('',#1936,0.34);
#603=VECTOR('',#1941,0.34);
#604=VECTOR('',#1946,0.34);
#605=VECTOR('',#1951,0.34);
#606=VECTOR('',#1956,0.34);
#607=VECTOR('',#1961,0.34);
#608=VECTOR('',#1966,0.34);
#609=VECTOR('',#1971,0.34);
#610=VECTOR('',#1976,0.34);
#611=VECTOR('',#1981,0.34);
#612=VECTOR('',#1986,0.34);
#613=VECTOR('',#1991,0.34);
#614=VECTOR('',#1996,0.34);
#615=VECTOR('',#2001,0.34);
#616=VECTOR('',#2006,0.34);
#617=VECTOR('',#2011,0.34);
#618=VECTOR('',#2016,0.34);
#619=VECTOR('',#2021,0.34);
#620=VECTOR('',#2026,0.34);
#621=VECTOR('',#2031,0.34);
#622=VECTOR('',#2034,1.);
#623=VECTOR('',#2035,1.);
#624=VECTOR('',#2038,1.);
#625=VECTOR('',#2039,1.);
#626=VECTOR('',#2042,1.);
#627=VECTOR('',#2051,0.34);
#628=VECTOR('',#2056,1.);
#629=VECTOR('',#2057,1.);
#630=VECTOR('',#2058,1.);
#631=VECTOR('',#2059,1.);
#632=VECTOR('',#2062,1.);
#633=VECTOR('',#2063,1.);
#634=VECTOR('',#2064,1.);
#635=VECTOR('',#2065,1.);
#636=VECTOR('',#2068,1.);
#637=VECTOR('',#2069,1.);
#638=VECTOR('',#2072,1.);
#639=VECTOR('',#2073,1.);
#640=VECTOR('',#2074,1.);
#641=VECTOR('',#2077,1.);
#642=VECTOR('',#2078,1.);
#643=VECTOR('',#2079,1.);
#644=VECTOR('',#2082,1.);
#645=VECTOR('',#2083,1.);
#646=VECTOR('',#2084,1.);
#647=VECTOR('',#2087,1.);
#648=VECTOR('',#2088,1.);
#649=VECTOR('',#2091,1.);
#650=VECTOR('',#2092,1.);
#651=VECTOR('',#2095,1.);
#652=VECTOR('',#2102,1.);
#653=VECTOR('',#2103,1.);
#654=VECTOR('',#2104,1.);
#655=VECTOR('',#2105,1.);
#656=VECTOR('',#2108,1.);
#657=VECTOR('',#2109,1.);
#658=VECTOR('',#2110,1.);
#659=VECTOR('',#2113,1.);
#660=VECTOR('',#2114,1.);
#661=VECTOR('',#2115,1.);
#662=VECTOR('',#2118,1.);
#663=VECTOR('',#2119,1.);
#664=VECTOR('',#2120,1.);
#665=VECTOR('',#2123,1.);
#666=VECTOR('',#2124,1.);
#667=VECTOR('',#2125,1.);
#668=VECTOR('',#2128,1.);
#669=VECTOR('',#2129,1.);
#670=VECTOR('',#2130,1.);
#671=VECTOR('',#2133,1.);
#672=VECTOR('',#2134,1.);
#673=VECTOR('',#2135,1.);
#674=VECTOR('',#2138,1.);
#675=VECTOR('',#2139,1.);
#676=VECTOR('',#2148,1.);
#677=VECTOR('',#2149,1.);
#678=VECTOR('',#2150,1.);
#679=VECTOR('',#2151,1.);
#680=VECTOR('',#2154,1.);
#681=VECTOR('',#2155,1.);
#682=VECTOR('',#2156,1.);
#683=VECTOR('',#2157,1.);
#684=VECTOR('',#2160,1.);
#685=VECTOR('',#2161,1.);
#686=VECTOR('',#2162,1.);
#687=VECTOR('',#2163,1.);
#688=VECTOR('',#2178,1.);
#689=VECTOR('',#2179,1.);
#690=VECTOR('',#2180,1.);
#691=VECTOR('',#2183,1.);
#692=VECTOR('',#2184,1.);
#693=VECTOR('',#2187,1.);
#694=VECTOR('',#2188,1.);
#695=VECTOR('',#2191,1.);
#696=VECTOR('',#2200,0.4);
#697=VECTOR('',#2213,0.42);
#698=VECTOR('',#2220,0.8);
#699=VECTOR('',#2231,0.734027674973257);
#700=VECTOR('',#2238,0.734027674973257);
#701=VECTOR('',#2241,1.);
#702=VECTOR('',#2242,1.);
#703=VECTOR('',#2245,1.);
#704=VECTOR('',#2248,1.);
#705=VECTOR('',#2253,0.4);
#706=VECTOR('',#2258,1.);
#707=VECTOR('',#2261,1.);
#708=VERTEX_POINT('',#2289);
#709=VERTEX_POINT('',#2290);
#710=VERTEX_POINT('',#2292);
#711=VERTEX_POINT('',#2294);
#712=VERTEX_POINT('',#2298);
#713=VERTEX_POINT('',#2300);
#714=VERTEX_POINT('',#2304);
#715=VERTEX_POINT('',#2305);
#716=VERTEX_POINT('',#2307);
#717=VERTEX_POINT('',#2309);
#718=VERTEX_POINT('',#2313);
#719=VERTEX_POINT('',#2315);
#720=VERTEX_POINT('',#2319);
#721=VERTEX_POINT('',#2321);
#722=VERTEX_POINT('',#2325);
#723=VERTEX_POINT('',#2327);
#724=VERTEX_POINT('',#2334);
#725=VERTEX_POINT('',#2336);
#726=VERTEX_POINT('',#2338);
#727=VERTEX_POINT('',#2340);
#728=VERTEX_POINT('',#2344);
#729=VERTEX_POINT('',#2347);
#730=VERTEX_POINT('',#2349);
#731=VERTEX_POINT('',#2351);
#732=VERTEX_POINT('',#2353);
#733=VERTEX_POINT('',#2355);
#734=VERTEX_POINT('',#2357);
#735=VERTEX_POINT('',#2359);
#736=VERTEX_POINT('',#2361);
#737=VERTEX_POINT('',#2363);
#738=VERTEX_POINT('',#2365);
#739=VERTEX_POINT('',#2368);
#740=VERTEX_POINT('',#2371);
#741=VERTEX_POINT('',#2373);
#742=VERTEX_POINT('',#2375);
#743=VERTEX_POINT('',#2377);
#744=VERTEX_POINT('',#2379);
#745=VERTEX_POINT('',#2381);
#746=VERTEX_POINT('',#2383);
#747=VERTEX_POINT('',#2385);
#748=VERTEX_POINT('',#2387);
#749=VERTEX_POINT('',#2389);
#750=VERTEX_POINT('',#2392);
#751=VERTEX_POINT('',#2396);
#752=VERTEX_POINT('',#2400);
#753=VERTEX_POINT('',#2404);
#754=VERTEX_POINT('',#2408);
#755=VERTEX_POINT('',#2412);
#756=VERTEX_POINT('',#2416);
#757=VERTEX_POINT('',#2420);
#758=VERTEX_POINT('',#2424);
#759=VERTEX_POINT('',#2428);
#760=VERTEX_POINT('',#2432);
#761=VERTEX_POINT('',#2436);
#762=VERTEX_POINT('',#2440);
#763=VERTEX_POINT('',#2444);
#764=VERTEX_POINT('',#2448);
#765=VERTEX_POINT('',#2452);
#766=VERTEX_POINT('',#2456);
#767=VERTEX_POINT('',#2460);
#768=VERTEX_POINT('',#2464);
#769=VERTEX_POINT('',#2468);
#770=VERTEX_POINT('',#2472);
#771=VERTEX_POINT('',#2476);
#772=VERTEX_POINT('',#2484);
#773=VERTEX_POINT('',#2486);
#774=VERTEX_POINT('',#2490);
#775=VERTEX_POINT('',#2491);
#776=VERTEX_POINT('',#2493);
#777=VERTEX_POINT('',#2495);
#778=VERTEX_POINT('',#2499);
#779=VERTEX_POINT('',#2500);
#780=VERTEX_POINT('',#2502);
#781=VERTEX_POINT('',#2504);
#782=VERTEX_POINT('',#2511);
#783=VERTEX_POINT('',#2513);
#784=VERTEX_POINT('',#2517);
#785=VERTEX_POINT('',#2519);
#786=VERTEX_POINT('',#2523);
#787=VERTEX_POINT('',#2524);
#788=VERTEX_POINT('',#2529);
#789=VERTEX_POINT('',#2533);
#790=VERTEX_POINT('',#2541);
#791=VERTEX_POINT('',#2542);
#792=VERTEX_POINT('',#2544);
#793=VERTEX_POINT('',#2546);
#794=VERTEX_POINT('',#2550);
#795=VERTEX_POINT('',#2552);
#796=VERTEX_POINT('',#2556);
#797=VERTEX_POINT('',#2558);
#798=VERTEX_POINT('',#2562);
#799=VERTEX_POINT('',#2564);
#800=VERTEX_POINT('',#2568);
#801=VERTEX_POINT('',#2570);
#802=VERTEX_POINT('',#2574);
#803=VERTEX_POINT('',#2576);
#804=VERTEX_POINT('',#2580);
#805=VERTEX_POINT('',#2582);
#806=VERTEX_POINT('',#2592);
#807=VERTEX_POINT('',#2593);
#808=VERTEX_POINT('',#2595);
#809=VERTEX_POINT('',#2597);
#810=VERTEX_POINT('',#2601);
#811=VERTEX_POINT('',#2602);
#812=VERTEX_POINT('',#2604);
#813=VERTEX_POINT('',#2606);
#814=VERTEX_POINT('',#2610);
#815=VERTEX_POINT('',#2611);
#816=VERTEX_POINT('',#2613);
#817=VERTEX_POINT('',#2615);
#818=VERTEX_POINT('',#2625);
#819=VERTEX_POINT('',#2627);
#820=VERTEX_POINT('',#2631);
#821=VERTEX_POINT('',#2635);
#822=VERTEX_POINT('',#2643);
#823=VERTEX_POINT('',#2645);
#824=VERTEX_POINT('',#2652);
#825=VERTEX_POINT('',#2654);
#826=VERTEX_POINT('',#2658);
#827=VERTEX_POINT('',#2660);
#828=VERTEX_POINT('',#2667);
#829=VERTEX_POINT('',#2668);
#830=VERTEX_POINT('',#2672);
#831=VERTEX_POINT('',#2676);
#832=VERTEX_POINT('',#2679);
#833=VERTEX_POINT('',#2683);
#834=VERTEX_POINT('',#2687);
#835=VERTEX_POINT('',#2695);
#836=VERTEX_POINT('',#2697);
#837=VERTEX_POINT('',#2699);
#838=VERTEX_POINT('',#2703);
#839=VERTEX_POINT('',#2707);
#840=VERTEX_POINT('',#2711);
#841=VERTEX_POINT('',#2715);
#842=VERTEX_POINT('',#2730);
#843=VERTEX_POINT('',#2732);
#844=EDGE_CURVE('',#708,#709,#434,.T.);
#845=EDGE_CURVE('',#710,#708,#435,.T.);
#846=EDGE_CURVE('',#711,#710,#436,.T.);
#847=EDGE_CURVE('',#709,#711,#437,.T.);
#848=EDGE_CURVE('',#712,#708,#438,.T.);
#849=EDGE_CURVE('',#713,#712,#439,.T.);
#850=EDGE_CURVE('',#710,#713,#440,.T.);
#851=EDGE_CURVE('',#714,#715,#441,.T.);
#852=EDGE_CURVE('',#716,#714,#442,.T.);
#853=EDGE_CURVE('',#717,#716,#443,.T.);
#854=EDGE_CURVE('',#717,#715,#444,.T.);
#855=EDGE_CURVE('',#715,#718,#445,.T.);
#856=EDGE_CURVE('',#719,#717,#446,.T.);
#857=EDGE_CURVE('',#719,#718,#447,.T.);
#858=EDGE_CURVE('',#718,#720,#448,.T.);
#859=EDGE_CURVE('',#721,#719,#449,.T.);
#860=EDGE_CURVE('',#721,#720,#450,.T.);
#861=EDGE_CURVE('',#720,#722,#451,.T.);
#862=EDGE_CURVE('',#723,#721,#452,.T.);
#863=EDGE_CURVE('',#723,#722,#453,.T.);
#864=EDGE_CURVE('',#722,#712,#454,.T.);
#865=EDGE_CURVE('',#713,#723,#455,.T.);
#866=EDGE_CURVE('',#724,#716,#456,.T.);
#867=EDGE_CURVE('',#725,#724,#457,.T.);
#868=EDGE_CURVE('',#725,#726,#458,.T.);
#869=EDGE_CURVE('',#726,#727,#459,.T.);
#870=EDGE_CURVE('',#711,#727,#460,.T.);
#871=EDGE_CURVE('',#714,#728,#461,.T.);
#872=EDGE_CURVE('',#728,#724,#462,.T.);
#873=EDGE_CURVE('',#729,#729,#164,.T.);
#874=EDGE_CURVE('',#730,#730,#165,.T.);
#875=EDGE_CURVE('',#731,#731,#166,.T.);
#876=EDGE_CURVE('',#732,#732,#167,.T.);
#877=EDGE_CURVE('',#733,#733,#168,.T.);
#878=EDGE_CURVE('',#734,#734,#169,.T.);
#879=EDGE_CURVE('',#735,#735,#170,.T.);
#880=EDGE_CURVE('',#736,#736,#171,.T.);
#881=EDGE_CURVE('',#737,#737,#172,.T.);
#882=EDGE_CURVE('',#738,#738,#173,.T.);
#883=EDGE_CURVE('',#727,#739,#463,.T.);
#884=EDGE_CURVE('',#739,#709,#464,.T.);
#885=EDGE_CURVE('',#740,#740,#174,.T.);
#886=EDGE_CURVE('',#741,#741,#175,.T.);
#887=EDGE_CURVE('',#742,#742,#176,.T.);
#888=EDGE_CURVE('',#743,#743,#177,.T.);
#889=EDGE_CURVE('',#744,#744,#178,.T.);
#890=EDGE_CURVE('',#745,#745,#179,.T.);
#891=EDGE_CURVE('',#746,#746,#180,.T.);
#892=EDGE_CURVE('',#747,#747,#181,.T.);
#893=EDGE_CURVE('',#748,#748,#182,.T.);
#894=EDGE_CURVE('',#749,#749,#183,.T.);
#895=EDGE_CURVE('',#750,#750,#184,.T.);
#896=EDGE_CURVE('',#750,#729,#465,.T.);
#897=EDGE_CURVE('',#751,#751,#185,.T.);
#898=EDGE_CURVE('',#751,#740,#466,.T.);
#899=EDGE_CURVE('',#752,#752,#186,.T.);
#900=EDGE_CURVE('',#752,#730,#467,.T.);
#901=EDGE_CURVE('',#753,#753,#187,.T.);
#902=EDGE_CURVE('',#753,#741,#468,.T.);
#903=EDGE_CURVE('',#754,#754,#188,.T.);
#904=EDGE_CURVE('',#754,#731,#469,.T.);
#905=EDGE_CURVE('',#755,#755,#189,.T.);
#906=EDGE_CURVE('',#755,#742,#470,.T.);
#907=EDGE_CURVE('',#756,#756,#190,.T.);
#908=EDGE_CURVE('',#756,#732,#471,.T.);
#909=EDGE_CURVE('',#757,#757,#191,.T.);
#910=EDGE_CURVE('',#757,#743,#472,.T.);
#911=EDGE_CURVE('',#758,#758,#192,.T.);
#912=EDGE_CURVE('',#758,#733,#473,.T.);
#913=EDGE_CURVE('',#759,#759,#193,.T.);
#914=EDGE_CURVE('',#759,#744,#474,.T.);
#915=EDGE_CURVE('',#760,#760,#194,.T.);
#916=EDGE_CURVE('',#760,#734,#475,.T.);
#917=EDGE_CURVE('',#761,#761,#195,.T.);
#918=EDGE_CURVE('',#761,#745,#476,.T.);
#919=EDGE_CURVE('',#762,#762,#196,.T.);
#920=EDGE_CURVE('',#762,#735,#477,.T.);
#921=EDGE_CURVE('',#763,#763,#197,.T.);
#922=EDGE_CURVE('',#763,#746,#478,.T.);
#923=EDGE_CURVE('',#764,#764,#198,.T.);
#924=EDGE_CURVE('',#764,#747,#479,.T.);
#925=EDGE_CURVE('',#765,#765,#199,.T.);
#926=EDGE_CURVE('',#765,#736,#480,.T.);
#927=EDGE_CURVE('',#766,#766,#200,.T.);
#928=EDGE_CURVE('',#766,#748,#481,.T.);
#929=EDGE_CURVE('',#767,#767,#201,.T.);
#930=EDGE_CURVE('',#767,#737,#482,.T.);
#931=EDGE_CURVE('',#768,#768,#202,.T.);
#932=EDGE_CURVE('',#768,#749,#483,.T.);
#933=EDGE_CURVE('',#769,#769,#203,.T.);
#934=EDGE_CURVE('',#769,#738,#484,.T.);
#935=EDGE_CURVE('',#770,#725,#485,.T.);
#936=EDGE_CURVE('',#770,#728,#486,.T.);
#937=EDGE_CURVE('',#771,#739,#487,.T.);
#938=EDGE_CURVE('',#771,#770,#488,.T.);
#939=EDGE_CURVE('',#726,#771,#489,.T.);
#940=EDGE_CURVE('',#772,#772,#204,.T.);
#941=EDGE_CURVE('',#772,#773,#490,.T.);
#942=EDGE_CURVE('',#773,#773,#205,.T.);
#943=EDGE_CURVE('',#774,#775,#491,.T.);
#944=EDGE_CURVE('',#774,#776,#492,.T.);
#945=EDGE_CURVE('',#777,#776,#493,.T.);
#946=EDGE_CURVE('',#775,#777,#494,.T.);
#947=EDGE_CURVE('',#778,#779,#495,.T.);
#948=EDGE_CURVE('',#778,#780,#496,.T.);
#949=EDGE_CURVE('',#781,#780,#497,.T.);
#950=EDGE_CURVE('',#779,#781,#498,.T.);
#951=EDGE_CURVE('',#776,#781,#499,.T.);
#952=EDGE_CURVE('',#780,#777,#500,.T.);
#953=EDGE_CURVE('',#775,#782,#501,.T.);
#954=EDGE_CURVE('',#782,#783,#502,.T.);
#955=EDGE_CURVE('',#783,#774,#503,.T.);
#956=EDGE_CURVE('',#779,#784,#504,.T.);
#957=EDGE_CURVE('',#784,#785,#505,.T.);
#958=EDGE_CURVE('',#785,#778,#506,.T.);
#959=EDGE_CURVE('',#786,#787,#507,.T.);
#960=EDGE_CURVE('',#787,#783,#508,.T.);
#961=EDGE_CURVE('',#786,#782,#509,.T.);
#962=EDGE_CURVE('',#788,#786,#510,.T.);
#963=EDGE_CURVE('',#788,#785,#511,.T.);
#964=EDGE_CURVE('',#789,#788,#512,.T.);
#965=EDGE_CURVE('',#789,#784,#513,.T.);
#966=EDGE_CURVE('',#787,#789,#514,.T.);
#967=EDGE_CURVE('',#790,#791,#515,.T.);
#968=EDGE_CURVE('',#790,#792,#516,.T.);
#969=EDGE_CURVE('',#793,#792,#517,.T.);
#970=EDGE_CURVE('',#791,#793,#518,.T.);
#971=EDGE_CURVE('',#791,#794,#519,.T.);
#972=EDGE_CURVE('',#795,#793,#520,.T.);
#973=EDGE_CURVE('',#794,#795,#521,.T.);
#974=EDGE_CURVE('',#794,#796,#522,.T.);
#975=EDGE_CURVE('',#797,#795,#523,.T.);
#976=EDGE_CURVE('',#796,#797,#524,.T.);
#977=EDGE_CURVE('',#796,#798,#525,.T.);
#978=EDGE_CURVE('',#799,#797,#526,.T.);
#979=EDGE_CURVE('',#798,#799,#527,.T.);
#980=EDGE_CURVE('',#798,#800,#528,.T.);
#981=EDGE_CURVE('',#801,#799,#529,.T.);
#982=EDGE_CURVE('',#800,#801,#530,.T.);
#983=EDGE_CURVE('',#800,#802,#531,.T.);
#984=EDGE_CURVE('',#803,#801,#532,.T.);
#985=EDGE_CURVE('',#802,#803,#533,.T.);
#986=EDGE_CURVE('',#802,#804,#534,.T.);
#987=EDGE_CURVE('',#805,#803,#535,.T.);
#988=EDGE_CURVE('',#804,#805,#536,.T.);
#989=EDGE_CURVE('',#804,#790,#537,.T.);
#990=EDGE_CURVE('',#792,#805,#538,.T.);
#991=EDGE_CURVE('',#806,#807,#539,.T.);
#992=EDGE_CURVE('',#808,#806,#540,.T.);
#993=EDGE_CURVE('',#809,#808,#541,.T.);
#994=EDGE_CURVE('',#809,#807,#542,.T.);
#995=EDGE_CURVE('',#810,#811,#543,.T.);
#996=EDGE_CURVE('',#812,#810,#544,.T.);
#997=EDGE_CURVE('',#813,#812,#545,.T.);
#998=EDGE_CURVE('',#811,#813,#546,.T.);
#999=EDGE_CURVE('',#814,#815,#547,.T.);
#1000=EDGE_CURVE('',#816,#814,#548,.T.);
#1001=EDGE_CURVE('',#817,#816,#549,.T.);
#1002=EDGE_CURVE('',#815,#817,#550,.T.);
#1003=EDGE_CURVE('',#807,#810,#206,.T.);
#1004=EDGE_CURVE('',#811,#806,#207,.T.);
#1005=EDGE_CURVE('',#812,#809,#208,.T.);
#1006=EDGE_CURVE('',#808,#813,#209,.T.);
#1007=EDGE_CURVE('',#814,#818,#551,.T.);
#1008=EDGE_CURVE('',#819,#818,#552,.T.);
#1009=EDGE_CURVE('',#816,#819,#553,.T.);
#1010=EDGE_CURVE('',#820,#819,#554,.T.);
#1011=EDGE_CURVE('',#817,#820,#555,.T.);
#1012=EDGE_CURVE('',#821,#820,#556,.T.);
#1013=EDGE_CURVE('',#815,#821,#557,.T.);
#1014=EDGE_CURVE('',#818,#821,#558,.T.);
#1015=EDGE_CURVE('',#822,#822,#210,.F.);
#1016=EDGE_CURVE('',#822,#823,#559,.T.);
#1017=EDGE_CURVE('',#823,#823,#211,.F.);
#1018=EDGE_CURVE('',#824,#824,#212,.T.);
#1019=EDGE_CURVE('',#824,#825,#560,.T.);
#1020=EDGE_CURVE('',#825,#825,#213,.T.);
#1021=EDGE_CURVE('',#826,#826,#214,.T.);
#1022=EDGE_CURVE('',#826,#827,#561,.T.);
#1023=EDGE_CURVE('',#827,#827,#215,.T.);
#1024=EDGE_CURVE('',#828,#829,#47,.T.);
#1025=EDGE_CURVE('',#830,#828,#48,.T.);
#1026=EDGE_CURVE('',#830,#831,#562,.T.);
#1027=EDGE_CURVE('',#831,#831,#216,.T.);
#1028=EDGE_CURVE('',#832,#830,#49,.T.);
#1029=EDGE_CURVE('',#833,#832,#50,.T.);
#1030=EDGE_CURVE('',#834,#833,#51,.T.);
#1031=EDGE_CURVE('',#829,#834,#52,.T.);
#1032=EDGE_CURVE('',#835,#835,#217,.T.);
#1033=EDGE_CURVE('',#835,#836,#563,.T.);
#1034=EDGE_CURVE('',#837,#836,#53,.T.);
#1035=EDGE_CURVE('',#838,#837,#54,.T.);
#1036=EDGE_CURVE('',#839,#838,#55,.T.);
#1037=EDGE_CURVE('',#840,#839,#56,.T.);
#1038=EDGE_CURVE('',#841,#840,#57,.T.);
#1039=EDGE_CURVE('',#836,#841,#58,.T.);
#1040=EDGE_CURVE('',#832,#841,#564,.T.);
#1041=EDGE_CURVE('',#833,#840,#565,.T.);
#1042=EDGE_CURVE('',#830,#836,#566,.T.);
#1043=EDGE_CURVE('',#828,#837,#567,.T.);
#1044=EDGE_CURVE('',#842,#842,#218,.F.);
#1045=EDGE_CURVE('',#842,#843,#568,.T.);
#1046=EDGE_CURVE('',#843,#843,#219,.F.);
#1047=EDGE_CURVE('',#829,#838,#569,.T.);
#1048=EDGE_CURVE('',#834,#839,#570,.T.);
#1049=ORIENTED_EDGE('',*,*,#844,.F.);
#1050=ORIENTED_EDGE('',*,*,#845,.F.);
#1051=ORIENTED_EDGE('',*,*,#846,.F.);
#1052=ORIENTED_EDGE('',*,*,#847,.F.);
#1053=ORIENTED_EDGE('',*,*,#848,.F.);
#1054=ORIENTED_EDGE('',*,*,#849,.F.);
#1055=ORIENTED_EDGE('',*,*,#850,.F.);
#1056=ORIENTED_EDGE('',*,*,#845,.T.);
#1057=ORIENTED_EDGE('',*,*,#851,.F.);
#1058=ORIENTED_EDGE('',*,*,#852,.F.);
#1059=ORIENTED_EDGE('',*,*,#853,.F.);
#1060=ORIENTED_EDGE('',*,*,#854,.T.);
#1061=ORIENTED_EDGE('',*,*,#855,.F.);
#1062=ORIENTED_EDGE('',*,*,#854,.F.);
#1063=ORIENTED_EDGE('',*,*,#856,.F.);
#1064=ORIENTED_EDGE('',*,*,#857,.T.);
#1065=ORIENTED_EDGE('',*,*,#858,.F.);
#1066=ORIENTED_EDGE('',*,*,#857,.F.);
#1067=ORIENTED_EDGE('',*,*,#859,.F.);
#1068=ORIENTED_EDGE('',*,*,#860,.T.);
#1069=ORIENTED_EDGE('',*,*,#861,.F.);
#1070=ORIENTED_EDGE('',*,*,#860,.F.);
#1071=ORIENTED_EDGE('',*,*,#862,.F.);
#1072=ORIENTED_EDGE('',*,*,#863,.T.);
#1073=ORIENTED_EDGE('',*,*,#864,.F.);
#1074=ORIENTED_EDGE('',*,*,#863,.F.);
#1075=ORIENTED_EDGE('',*,*,#865,.F.);
#1076=ORIENTED_EDGE('',*,*,#849,.T.);
#1077=ORIENTED_EDGE('',*,*,#846,.T.);
#1078=ORIENTED_EDGE('',*,*,#850,.T.);
#1079=ORIENTED_EDGE('',*,*,#865,.T.);
#1080=ORIENTED_EDGE('',*,*,#862,.T.);
#1081=ORIENTED_EDGE('',*,*,#859,.T.);
#1082=ORIENTED_EDGE('',*,*,#856,.T.);
#1083=ORIENTED_EDGE('',*,*,#853,.T.);
#1084=ORIENTED_EDGE('',*,*,#866,.F.);
#1085=ORIENTED_EDGE('',*,*,#867,.F.);
#1086=ORIENTED_EDGE('',*,*,#868,.T.);
#1087=ORIENTED_EDGE('',*,*,#869,.T.);
#1088=ORIENTED_EDGE('',*,*,#870,.F.);
#1089=ORIENTED_EDGE('',*,*,#852,.T.);
#1090=ORIENTED_EDGE('',*,*,#871,.T.);
#1091=ORIENTED_EDGE('',*,*,#872,.T.);
#1092=ORIENTED_EDGE('',*,*,#866,.T.);
#1093=ORIENTED_EDGE('',*,*,#873,.T.);
#1094=ORIENTED_EDGE('',*,*,#874,.T.);
#1095=ORIENTED_EDGE('',*,*,#875,.T.);
#1096=ORIENTED_EDGE('',*,*,#876,.T.);
#1097=ORIENTED_EDGE('',*,*,#877,.T.);
#1098=ORIENTED_EDGE('',*,*,#878,.T.);
#1099=ORIENTED_EDGE('',*,*,#879,.T.);
#1100=ORIENTED_EDGE('',*,*,#880,.T.);
#1101=ORIENTED_EDGE('',*,*,#881,.T.);
#1102=ORIENTED_EDGE('',*,*,#882,.T.);
#1103=ORIENTED_EDGE('',*,*,#847,.T.);
#1104=ORIENTED_EDGE('',*,*,#870,.T.);
#1105=ORIENTED_EDGE('',*,*,#883,.T.);
#1106=ORIENTED_EDGE('',*,*,#884,.T.);
#1107=ORIENTED_EDGE('',*,*,#885,.T.);
#1108=ORIENTED_EDGE('',*,*,#886,.T.);
#1109=ORIENTED_EDGE('',*,*,#887,.T.);
#1110=ORIENTED_EDGE('',*,*,#888,.T.);
#1111=ORIENTED_EDGE('',*,*,#889,.T.);
#1112=ORIENTED_EDGE('',*,*,#890,.T.);
#1113=ORIENTED_EDGE('',*,*,#891,.T.);
#1114=ORIENTED_EDGE('',*,*,#892,.T.);
#1115=ORIENTED_EDGE('',*,*,#893,.T.);
#1116=ORIENTED_EDGE('',*,*,#894,.T.);
#1117=ORIENTED_EDGE('',*,*,#895,.F.);
#1118=ORIENTED_EDGE('',*,*,#896,.T.);
#1119=ORIENTED_EDGE('',*,*,#873,.F.);
#1120=ORIENTED_EDGE('',*,*,#896,.F.);
#1121=ORIENTED_EDGE('',*,*,#897,.F.);
#1122=ORIENTED_EDGE('',*,*,#898,.T.);
#1123=ORIENTED_EDGE('',*,*,#885,.F.);
#1124=ORIENTED_EDGE('',*,*,#898,.F.);
#1125=ORIENTED_EDGE('',*,*,#899,.F.);
#1126=ORIENTED_EDGE('',*,*,#900,.T.);
#1127=ORIENTED_EDGE('',*,*,#874,.F.);
#1128=ORIENTED_EDGE('',*,*,#900,.F.);
#1129=ORIENTED_EDGE('',*,*,#901,.F.);
#1130=ORIENTED_EDGE('',*,*,#902,.T.);
#1131=ORIENTED_EDGE('',*,*,#886,.F.);
#1132=ORIENTED_EDGE('',*,*,#902,.F.);
#1133=ORIENTED_EDGE('',*,*,#903,.F.);
#1134=ORIENTED_EDGE('',*,*,#904,.T.);
#1135=ORIENTED_EDGE('',*,*,#875,.F.);
#1136=ORIENTED_EDGE('',*,*,#904,.F.);
#1137=ORIENTED_EDGE('',*,*,#905,.F.);
#1138=ORIENTED_EDGE('',*,*,#906,.T.);
#1139=ORIENTED_EDGE('',*,*,#887,.F.);
#1140=ORIENTED_EDGE('',*,*,#906,.F.);
#1141=ORIENTED_EDGE('',*,*,#907,.F.);
#1142=ORIENTED_EDGE('',*,*,#908,.T.);
#1143=ORIENTED_EDGE('',*,*,#876,.F.);
#1144=ORIENTED_EDGE('',*,*,#908,.F.);
#1145=ORIENTED_EDGE('',*,*,#909,.F.);
#1146=ORIENTED_EDGE('',*,*,#910,.T.);
#1147=ORIENTED_EDGE('',*,*,#888,.F.);
#1148=ORIENTED_EDGE('',*,*,#910,.F.);
#1149=ORIENTED_EDGE('',*,*,#911,.F.);
#1150=ORIENTED_EDGE('',*,*,#912,.T.);
#1151=ORIENTED_EDGE('',*,*,#877,.F.);
#1152=ORIENTED_EDGE('',*,*,#912,.F.);
#1153=ORIENTED_EDGE('',*,*,#913,.F.);
#1154=ORIENTED_EDGE('',*,*,#914,.T.);
#1155=ORIENTED_EDGE('',*,*,#889,.F.);
#1156=ORIENTED_EDGE('',*,*,#914,.F.);
#1157=ORIENTED_EDGE('',*,*,#915,.F.);
#1158=ORIENTED_EDGE('',*,*,#916,.T.);
#1159=ORIENTED_EDGE('',*,*,#878,.F.);
#1160=ORIENTED_EDGE('',*,*,#916,.F.);
#1161=ORIENTED_EDGE('',*,*,#917,.F.);
#1162=ORIENTED_EDGE('',*,*,#918,.T.);
#1163=ORIENTED_EDGE('',*,*,#890,.F.);
#1164=ORIENTED_EDGE('',*,*,#918,.F.);
#1165=ORIENTED_EDGE('',*,*,#919,.F.);
#1166=ORIENTED_EDGE('',*,*,#920,.T.);
#1167=ORIENTED_EDGE('',*,*,#879,.F.);
#1168=ORIENTED_EDGE('',*,*,#920,.F.);
#1169=ORIENTED_EDGE('',*,*,#921,.F.);
#1170=ORIENTED_EDGE('',*,*,#922,.T.);
#1171=ORIENTED_EDGE('',*,*,#891,.F.);
#1172=ORIENTED_EDGE('',*,*,#922,.F.);
#1173=ORIENTED_EDGE('',*,*,#923,.F.);
#1174=ORIENTED_EDGE('',*,*,#924,.T.);
#1175=ORIENTED_EDGE('',*,*,#892,.F.);
#1176=ORIENTED_EDGE('',*,*,#924,.F.);
#1177=ORIENTED_EDGE('',*,*,#925,.F.);
#1178=ORIENTED_EDGE('',*,*,#926,.T.);
#1179=ORIENTED_EDGE('',*,*,#880,.F.);
#1180=ORIENTED_EDGE('',*,*,#926,.F.);
#1181=ORIENTED_EDGE('',*,*,#927,.F.);
#1182=ORIENTED_EDGE('',*,*,#928,.T.);
#1183=ORIENTED_EDGE('',*,*,#893,.F.);
#1184=ORIENTED_EDGE('',*,*,#928,.F.);
#1185=ORIENTED_EDGE('',*,*,#929,.F.);
#1186=ORIENTED_EDGE('',*,*,#930,.T.);
#1187=ORIENTED_EDGE('',*,*,#881,.F.);
#1188=ORIENTED_EDGE('',*,*,#930,.F.);
#1189=ORIENTED_EDGE('',*,*,#931,.F.);
#1190=ORIENTED_EDGE('',*,*,#932,.T.);
#1191=ORIENTED_EDGE('',*,*,#894,.F.);
#1192=ORIENTED_EDGE('',*,*,#932,.F.);
#1193=ORIENTED_EDGE('',*,*,#933,.F.);
#1194=ORIENTED_EDGE('',*,*,#934,.T.);
#1195=ORIENTED_EDGE('',*,*,#882,.F.);
#1196=ORIENTED_EDGE('',*,*,#934,.F.);
#1197=ORIENTED_EDGE('',*,*,#935,.T.);
#1198=ORIENTED_EDGE('',*,*,#867,.T.);
#1199=ORIENTED_EDGE('',*,*,#872,.F.);
#1200=ORIENTED_EDGE('',*,*,#936,.F.);
#1201=ORIENTED_EDGE('',*,*,#844,.T.);
#1202=ORIENTED_EDGE('',*,*,#884,.F.);
#1203=ORIENTED_EDGE('',*,*,#937,.F.);
#1204=ORIENTED_EDGE('',*,*,#938,.T.);
#1205=ORIENTED_EDGE('',*,*,#936,.T.);
#1206=ORIENTED_EDGE('',*,*,#871,.F.);
#1207=ORIENTED_EDGE('',*,*,#851,.T.);
#1208=ORIENTED_EDGE('',*,*,#855,.T.);
#1209=ORIENTED_EDGE('',*,*,#858,.T.);
#1210=ORIENTED_EDGE('',*,*,#861,.T.);
#1211=ORIENTED_EDGE('',*,*,#864,.T.);
#1212=ORIENTED_EDGE('',*,*,#848,.T.);
#1213=ORIENTED_EDGE('',*,*,#939,.T.);
#1214=ORIENTED_EDGE('',*,*,#937,.T.);
#1215=ORIENTED_EDGE('',*,*,#883,.F.);
#1216=ORIENTED_EDGE('',*,*,#869,.F.);
#1217=ORIENTED_EDGE('',*,*,#868,.F.);
#1218=ORIENTED_EDGE('',*,*,#935,.F.);
#1219=ORIENTED_EDGE('',*,*,#938,.F.);
#1220=ORIENTED_EDGE('',*,*,#939,.F.);
#1221=ORIENTED_EDGE('',*,*,#933,.T.);
#1222=ORIENTED_EDGE('',*,*,#931,.T.);
#1223=ORIENTED_EDGE('',*,*,#929,.T.);
#1224=ORIENTED_EDGE('',*,*,#927,.T.);
#1225=ORIENTED_EDGE('',*,*,#925,.T.);
#1226=ORIENTED_EDGE('',*,*,#923,.T.);
#1227=ORIENTED_EDGE('',*,*,#921,.T.);
#1228=ORIENTED_EDGE('',*,*,#919,.T.);
#1229=ORIENTED_EDGE('',*,*,#917,.T.);
#1230=ORIENTED_EDGE('',*,*,#915,.T.);
#1231=ORIENTED_EDGE('',*,*,#913,.T.);
#1232=ORIENTED_EDGE('',*,*,#911,.T.);
#1233=ORIENTED_EDGE('',*,*,#909,.T.);
#1234=ORIENTED_EDGE('',*,*,#907,.T.);
#1235=ORIENTED_EDGE('',*,*,#905,.T.);
#1236=ORIENTED_EDGE('',*,*,#903,.T.);
#1237=ORIENTED_EDGE('',*,*,#901,.T.);
#1238=ORIENTED_EDGE('',*,*,#899,.T.);
#1239=ORIENTED_EDGE('',*,*,#897,.T.);
#1240=ORIENTED_EDGE('',*,*,#895,.T.);
#1241=ORIENTED_EDGE('',*,*,#940,.F.);
#1242=ORIENTED_EDGE('',*,*,#941,.T.);
#1243=ORIENTED_EDGE('',*,*,#942,.F.);
#1244=ORIENTED_EDGE('',*,*,#941,.F.);
#1245=ORIENTED_EDGE('',*,*,#943,.F.);
#1246=ORIENTED_EDGE('',*,*,#944,.T.);
#1247=ORIENTED_EDGE('',*,*,#945,.F.);
#1248=ORIENTED_EDGE('',*,*,#946,.F.);
#1249=ORIENTED_EDGE('',*,*,#947,.F.);
#1250=ORIENTED_EDGE('',*,*,#948,.T.);
#1251=ORIENTED_EDGE('',*,*,#949,.F.);
#1252=ORIENTED_EDGE('',*,*,#950,.F.);
#1253=ORIENTED_EDGE('',*,*,#951,.T.);
#1254=ORIENTED_EDGE('',*,*,#949,.T.);
#1255=ORIENTED_EDGE('',*,*,#952,.T.);
#1256=ORIENTED_EDGE('',*,*,#945,.T.);
#1257=ORIENTED_EDGE('',*,*,#942,.T.);
#1258=ORIENTED_EDGE('',*,*,#943,.T.);
#1259=ORIENTED_EDGE('',*,*,#953,.T.);
#1260=ORIENTED_EDGE('',*,*,#954,.T.);
#1261=ORIENTED_EDGE('',*,*,#955,.T.);
#1262=ORIENTED_EDGE('',*,*,#947,.T.);
#1263=ORIENTED_EDGE('',*,*,#956,.T.);
#1264=ORIENTED_EDGE('',*,*,#957,.T.);
#1265=ORIENTED_EDGE('',*,*,#958,.T.);
#1266=ORIENTED_EDGE('',*,*,#959,.T.);
#1267=ORIENTED_EDGE('',*,*,#960,.T.);
#1268=ORIENTED_EDGE('',*,*,#954,.F.);
#1269=ORIENTED_EDGE('',*,*,#961,.F.);
#1270=ORIENTED_EDGE('',*,*,#962,.T.);
#1271=ORIENTED_EDGE('',*,*,#961,.T.);
#1272=ORIENTED_EDGE('',*,*,#953,.F.);
#1273=ORIENTED_EDGE('',*,*,#946,.T.);
#1274=ORIENTED_EDGE('',*,*,#952,.F.);
#1275=ORIENTED_EDGE('',*,*,#948,.F.);
#1276=ORIENTED_EDGE('',*,*,#958,.F.);
#1277=ORIENTED_EDGE('',*,*,#963,.F.);
#1278=ORIENTED_EDGE('',*,*,#964,.T.);
#1279=ORIENTED_EDGE('',*,*,#963,.T.);
#1280=ORIENTED_EDGE('',*,*,#957,.F.);
#1281=ORIENTED_EDGE('',*,*,#965,.F.);
#1282=ORIENTED_EDGE('',*,*,#966,.T.);
#1283=ORIENTED_EDGE('',*,*,#965,.T.);
#1284=ORIENTED_EDGE('',*,*,#956,.F.);
#1285=ORIENTED_EDGE('',*,*,#950,.T.);
#1286=ORIENTED_EDGE('',*,*,#951,.F.);
#1287=ORIENTED_EDGE('',*,*,#944,.F.);
#1288=ORIENTED_EDGE('',*,*,#955,.F.);
#1289=ORIENTED_EDGE('',*,*,#960,.F.);
#1290=ORIENTED_EDGE('',*,*,#966,.F.);
#1291=ORIENTED_EDGE('',*,*,#959,.F.);
#1292=ORIENTED_EDGE('',*,*,#962,.F.);
#1293=ORIENTED_EDGE('',*,*,#964,.F.);
#1294=ORIENTED_EDGE('',*,*,#940,.T.);
#1295=ORIENTED_EDGE('',*,*,#967,.F.);
#1296=ORIENTED_EDGE('',*,*,#968,.T.);
#1297=ORIENTED_EDGE('',*,*,#969,.F.);
#1298=ORIENTED_EDGE('',*,*,#970,.F.);
#1299=ORIENTED_EDGE('',*,*,#971,.F.);
#1300=ORIENTED_EDGE('',*,*,#970,.T.);
#1301=ORIENTED_EDGE('',*,*,#972,.F.);
#1302=ORIENTED_EDGE('',*,*,#973,.F.);
#1303=ORIENTED_EDGE('',*,*,#974,.F.);
#1304=ORIENTED_EDGE('',*,*,#973,.T.);
#1305=ORIENTED_EDGE('',*,*,#975,.F.);
#1306=ORIENTED_EDGE('',*,*,#976,.F.);
#1307=ORIENTED_EDGE('',*,*,#977,.F.);
#1308=ORIENTED_EDGE('',*,*,#976,.T.);
#1309=ORIENTED_EDGE('',*,*,#978,.F.);
#1310=ORIENTED_EDGE('',*,*,#979,.F.);
#1311=ORIENTED_EDGE('',*,*,#980,.F.);
#1312=ORIENTED_EDGE('',*,*,#979,.T.);
#1313=ORIENTED_EDGE('',*,*,#981,.F.);
#1314=ORIENTED_EDGE('',*,*,#982,.F.);
#1315=ORIENTED_EDGE('',*,*,#983,.F.);
#1316=ORIENTED_EDGE('',*,*,#982,.T.);
#1317=ORIENTED_EDGE('',*,*,#984,.F.);
#1318=ORIENTED_EDGE('',*,*,#985,.F.);
#1319=ORIENTED_EDGE('',*,*,#986,.F.);
#1320=ORIENTED_EDGE('',*,*,#985,.T.);
#1321=ORIENTED_EDGE('',*,*,#987,.F.);
#1322=ORIENTED_EDGE('',*,*,#988,.F.);
#1323=ORIENTED_EDGE('',*,*,#989,.F.);
#1324=ORIENTED_EDGE('',*,*,#988,.T.);
#1325=ORIENTED_EDGE('',*,*,#990,.F.);
#1326=ORIENTED_EDGE('',*,*,#968,.F.);
#1327=ORIENTED_EDGE('',*,*,#990,.T.);
#1328=ORIENTED_EDGE('',*,*,#987,.T.);
#1329=ORIENTED_EDGE('',*,*,#984,.T.);
#1330=ORIENTED_EDGE('',*,*,#981,.T.);
#1331=ORIENTED_EDGE('',*,*,#978,.T.);
#1332=ORIENTED_EDGE('',*,*,#975,.T.);
#1333=ORIENTED_EDGE('',*,*,#972,.T.);
#1334=ORIENTED_EDGE('',*,*,#969,.T.);
#1335=ORIENTED_EDGE('',*,*,#989,.T.);
#1336=ORIENTED_EDGE('',*,*,#967,.T.);
#1337=ORIENTED_EDGE('',*,*,#971,.T.);
#1338=ORIENTED_EDGE('',*,*,#974,.T.);
#1339=ORIENTED_EDGE('',*,*,#977,.T.);
#1340=ORIENTED_EDGE('',*,*,#980,.T.);
#1341=ORIENTED_EDGE('',*,*,#983,.T.);
#1342=ORIENTED_EDGE('',*,*,#986,.T.);
#1343=ORIENTED_EDGE('',*,*,#991,.F.);
#1344=ORIENTED_EDGE('',*,*,#992,.F.);
#1345=ORIENTED_EDGE('',*,*,#993,.F.);
#1346=ORIENTED_EDGE('',*,*,#994,.T.);
#1347=ORIENTED_EDGE('',*,*,#995,.F.);
#1348=ORIENTED_EDGE('',*,*,#996,.F.);
#1349=ORIENTED_EDGE('',*,*,#997,.F.);
#1350=ORIENTED_EDGE('',*,*,#998,.F.);
#1351=ORIENTED_EDGE('',*,*,#999,.F.);
#1352=ORIENTED_EDGE('',*,*,#1000,.F.);
#1353=ORIENTED_EDGE('',*,*,#1001,.F.);
#1354=ORIENTED_EDGE('',*,*,#1002,.F.);
#1355=ORIENTED_EDGE('',*,*,#991,.T.);
#1356=ORIENTED_EDGE('',*,*,#1003,.T.);
#1357=ORIENTED_EDGE('',*,*,#995,.T.);
#1358=ORIENTED_EDGE('',*,*,#1004,.T.);
#1359=ORIENTED_EDGE('',*,*,#994,.F.);
#1360=ORIENTED_EDGE('',*,*,#1005,.F.);
#1361=ORIENTED_EDGE('',*,*,#996,.T.);
#1362=ORIENTED_EDGE('',*,*,#1003,.F.);
#1363=ORIENTED_EDGE('',*,*,#992,.T.);
#1364=ORIENTED_EDGE('',*,*,#1004,.F.);
#1365=ORIENTED_EDGE('',*,*,#998,.T.);
#1366=ORIENTED_EDGE('',*,*,#1006,.F.);
#1367=ORIENTED_EDGE('',*,*,#1000,.T.);
#1368=ORIENTED_EDGE('',*,*,#1007,.T.);
#1369=ORIENTED_EDGE('',*,*,#1008,.F.);
#1370=ORIENTED_EDGE('',*,*,#1009,.F.);
#1371=ORIENTED_EDGE('',*,*,#1001,.T.);
#1372=ORIENTED_EDGE('',*,*,#1009,.T.);
#1373=ORIENTED_EDGE('',*,*,#1010,.F.);
#1374=ORIENTED_EDGE('',*,*,#1011,.F.);
#1375=ORIENTED_EDGE('',*,*,#1002,.T.);
#1376=ORIENTED_EDGE('',*,*,#1011,.T.);
#1377=ORIENTED_EDGE('',*,*,#1012,.F.);
#1378=ORIENTED_EDGE('',*,*,#1013,.F.);
#1379=ORIENTED_EDGE('',*,*,#999,.T.);
#1380=ORIENTED_EDGE('',*,*,#1013,.T.);
#1381=ORIENTED_EDGE('',*,*,#1014,.F.);
#1382=ORIENTED_EDGE('',*,*,#1007,.F.);
#1383=ORIENTED_EDGE('',*,*,#1014,.T.);
#1384=ORIENTED_EDGE('',*,*,#1012,.T.);
#1385=ORIENTED_EDGE('',*,*,#1010,.T.);
#1386=ORIENTED_EDGE('',*,*,#1008,.T.);
#1387=ORIENTED_EDGE('',*,*,#993,.T.);
#1388=ORIENTED_EDGE('',*,*,#1006,.T.);
#1389=ORIENTED_EDGE('',*,*,#997,.T.);
#1390=ORIENTED_EDGE('',*,*,#1005,.T.);
#1391=ORIENTED_EDGE('',*,*,#1015,.F.);
#1392=ORIENTED_EDGE('',*,*,#1016,.T.);
#1393=ORIENTED_EDGE('',*,*,#1017,.T.);
#1394=ORIENTED_EDGE('',*,*,#1016,.F.);
#1395=ORIENTED_EDGE('',*,*,#1015,.T.);
#1396=ORIENTED_EDGE('',*,*,#1017,.F.);
#1397=ORIENTED_EDGE('',*,*,#1018,.F.);
#1398=ORIENTED_EDGE('',*,*,#1019,.T.);
#1399=ORIENTED_EDGE('',*,*,#1020,.T.);
#1400=ORIENTED_EDGE('',*,*,#1019,.F.);
#1401=ORIENTED_EDGE('',*,*,#1021,.F.);
#1402=ORIENTED_EDGE('',*,*,#1022,.T.);
#1403=ORIENTED_EDGE('',*,*,#1023,.T.);
#1404=ORIENTED_EDGE('',*,*,#1022,.F.);
#1405=ORIENTED_EDGE('',*,*,#1021,.T.);
#1406=ORIENTED_EDGE('',*,*,#1018,.T.);
#1407=ORIENTED_EDGE('',*,*,#1023,.F.);
#1408=ORIENTED_EDGE('',*,*,#1020,.F.);
#1409=ORIENTED_EDGE('',*,*,#1024,.F.);
#1410=ORIENTED_EDGE('',*,*,#1025,.F.);
#1411=ORIENTED_EDGE('',*,*,#1026,.T.);
#1412=ORIENTED_EDGE('',*,*,#1027,.F.);
#1413=ORIENTED_EDGE('',*,*,#1026,.F.);
#1414=ORIENTED_EDGE('',*,*,#1028,.F.);
#1415=ORIENTED_EDGE('',*,*,#1029,.F.);
#1416=ORIENTED_EDGE('',*,*,#1030,.F.);
#1417=ORIENTED_EDGE('',*,*,#1031,.F.);
#1418=ORIENTED_EDGE('',*,*,#1032,.F.);
#1419=ORIENTED_EDGE('',*,*,#1033,.T.);
#1420=ORIENTED_EDGE('',*,*,#1034,.F.);
#1421=ORIENTED_EDGE('',*,*,#1035,.F.);
#1422=ORIENTED_EDGE('',*,*,#1036,.F.);
#1423=ORIENTED_EDGE('',*,*,#1037,.F.);
#1424=ORIENTED_EDGE('',*,*,#1038,.F.);
#1425=ORIENTED_EDGE('',*,*,#1039,.F.);
#1426=ORIENTED_EDGE('',*,*,#1033,.F.);
#1427=ORIENTED_EDGE('',*,*,#1029,.T.);
#1428=ORIENTED_EDGE('',*,*,#1040,.T.);
#1429=ORIENTED_EDGE('',*,*,#1038,.T.);
#1430=ORIENTED_EDGE('',*,*,#1041,.F.);
#1431=ORIENTED_EDGE('',*,*,#1028,.T.);
#1432=ORIENTED_EDGE('',*,*,#1042,.T.);
#1433=ORIENTED_EDGE('',*,*,#1039,.T.);
#1434=ORIENTED_EDGE('',*,*,#1040,.F.);
#1435=ORIENTED_EDGE('',*,*,#1025,.T.);
#1436=ORIENTED_EDGE('',*,*,#1043,.T.);
#1437=ORIENTED_EDGE('',*,*,#1034,.T.);
#1438=ORIENTED_EDGE('',*,*,#1042,.F.);
#1439=ORIENTED_EDGE('',*,*,#1044,.F.);
#1440=ORIENTED_EDGE('',*,*,#1045,.T.);
#1441=ORIENTED_EDGE('',*,*,#1046,.T.);
#1442=ORIENTED_EDGE('',*,*,#1045,.F.);
#1443=ORIENTED_EDGE('',*,*,#1024,.T.);
#1444=ORIENTED_EDGE('',*,*,#1047,.T.);
#1445=ORIENTED_EDGE('',*,*,#1035,.T.);
#1446=ORIENTED_EDGE('',*,*,#1043,.F.);
#1447=ORIENTED_EDGE('',*,*,#1030,.T.);
#1448=ORIENTED_EDGE('',*,*,#1041,.T.);
#1449=ORIENTED_EDGE('',*,*,#1037,.T.);
#1450=ORIENTED_EDGE('',*,*,#1048,.F.);
#1451=ORIENTED_EDGE('',*,*,#1031,.T.);
#1452=ORIENTED_EDGE('',*,*,#1048,.T.);
#1453=ORIENTED_EDGE('',*,*,#1036,.T.);
#1454=ORIENTED_EDGE('',*,*,#1047,.F.);
#1455=ORIENTED_EDGE('',*,*,#1032,.T.);
#1456=ORIENTED_EDGE('',*,*,#1044,.T.);
#1457=ORIENTED_EDGE('',*,*,#1027,.T.);
#1458=ORIENTED_EDGE('',*,*,#1046,.F.);
#1459=PLANE('',#1683);
#1460=PLANE('',#1684);
#1461=PLANE('',#1685);
#1462=PLANE('',#1686);
#1463=PLANE('',#1687);
#1464=PLANE('',#1688);
#1465=PLANE('',#1689);
#1466=PLANE('',#1690);
#1467=PLANE('',#1691);
#1468=PLANE('',#1702);
#1469=PLANE('',#1753);
#1470=PLANE('',#1754);
#1471=PLANE('',#1755);
#1472=PLANE('',#1756);
#1473=PLANE('',#1761);
#1474=PLANE('',#1762);
#1475=PLANE('',#1763);
#1476=PLANE('',#1764);
#1477=PLANE('',#1765);
#1478=PLANE('',#1766);
#1479=PLANE('',#1767);
#1480=PLANE('',#1768);
#1481=PLANE('',#1769);
#1482=PLANE('',#1770);
#1483=PLANE('',#1772);
#1484=PLANE('',#1773);
#1485=PLANE('',#1774);
#1486=PLANE('',#1775);
#1487=PLANE('',#1776);
#1488=PLANE('',#1777);
#1489=PLANE('',#1778);
#1490=PLANE('',#1779);
#1491=PLANE('',#1780);
#1492=PLANE('',#1781);
#1493=PLANE('',#1783);
#1494=PLANE('',#1784);
#1495=PLANE('',#1785);
#1496=PLANE('',#1792);
#1497=PLANE('',#1793);
#1498=PLANE('',#1794);
#1499=PLANE('',#1795);
#1500=PLANE('',#1796);
#1501=PLANE('',#1801);
#1502=PLANE('',#1802);
#1503=PLANE('',#1810);
#1504=PLANE('',#1811);
#1505=PLANE('',#1817);
#1506=PLANE('',#1818);
#1507=PLANE('',#1819);
#1508=PLANE('',#1823);
#1509=PLANE('',#1824);
#1510=PLANE('',#1825);
#1511=PLANE('',#1826);
#1512=PLANE('',#1827);
#1513=ADVANCED_FACE('',(#220),#1459,.F.);
#1514=ADVANCED_FACE('',(#221),#1460,.F.);
#1515=ADVANCED_FACE('',(#222),#1461,.F.);
#1516=ADVANCED_FACE('',(#223),#1462,.F.);
#1517=ADVANCED_FACE('',(#224),#1463,.F.);
#1518=ADVANCED_FACE('',(#225),#1464,.F.);
#1519=ADVANCED_FACE('',(#226),#1465,.F.);
#1520=ADVANCED_FACE('',(#227),#1466,.T.);
#1521=ADVANCED_FACE('',(#228,#116,#117,#118,#119,#120,#121,#122,#123,#124,
#125),#1467,.T.);
#1522=ADVANCED_FACE('',(#229,#126,#127,#128,#129,#130,#131,#132,#133,#134,
#135),#1468,.T.);
#1523=ADVANCED_FACE('',(#230),#89,.F.);
#1524=ADVANCED_FACE('',(#231),#90,.F.);
#1525=ADVANCED_FACE('',(#232),#91,.F.);
#1526=ADVANCED_FACE('',(#233),#92,.F.);
#1527=ADVANCED_FACE('',(#234),#93,.F.);
#1528=ADVANCED_FACE('',(#235),#94,.F.);
#1529=ADVANCED_FACE('',(#236),#95,.F.);
#1530=ADVANCED_FACE('',(#237),#96,.F.);
#1531=ADVANCED_FACE('',(#238),#97,.F.);
#1532=ADVANCED_FACE('',(#239),#98,.F.);
#1533=ADVANCED_FACE('',(#240),#99,.F.);
#1534=ADVANCED_FACE('',(#241),#100,.F.);
#1535=ADVANCED_FACE('',(#242),#101,.F.);
#1536=ADVANCED_FACE('',(#243),#102,.F.);
#1537=ADVANCED_FACE('',(#244),#103,.F.);
#1538=ADVANCED_FACE('',(#245),#104,.F.);
#1539=ADVANCED_FACE('',(#246),#105,.F.);
#1540=ADVANCED_FACE('',(#247),#106,.F.);
#1541=ADVANCED_FACE('',(#248),#107,.F.);
#1542=ADVANCED_FACE('',(#249),#108,.F.);
#1543=ADVANCED_FACE('',(#250),#1469,.T.);
#1544=ADVANCED_FACE('',(#251),#1470,.T.);
#1545=ADVANCED_FACE('',(#252),#1471,.T.);
#1546=ADVANCED_FACE('',(#253,#136,#137,#138,#139,#140,#141,#142,#143,#144,
#145,#146,#147,#148,#149,#150,#151,#152,#153,#154,#155),#1472,.F.);
#1547=ADVANCED_FACE('',(#254),#109,.F.);
#1548=ADVANCED_FACE('',(#255),#1473,.T.);
#1549=ADVANCED_FACE('',(#256),#1474,.T.);
#1550=ADVANCED_FACE('',(#257,#156),#1475,.T.);
#1551=ADVANCED_FACE('',(#258),#1476,.T.);
#1552=ADVANCED_FACE('',(#259),#1477,.T.);
#1553=ADVANCED_FACE('',(#260),#1478,.T.);
#1554=ADVANCED_FACE('',(#261),#1479,.T.);
#1555=ADVANCED_FACE('',(#262),#1480,.T.);
#1556=ADVANCED_FACE('',(#263),#1481,.T.);
#1557=ADVANCED_FACE('',(#264,#157),#1482,.F.);
#1558=ADVANCED_FACE('',(#265),#1483,.T.);
#1559=ADVANCED_FACE('',(#266),#1484,.T.);
#1560=ADVANCED_FACE('',(#267),#1485,.T.);
#1561=ADVANCED_FACE('',(#268),#1486,.T.);
#1562=ADVANCED_FACE('',(#269),#1487,.T.);
#1563=ADVANCED_FACE('',(#270),#1488,.T.);
#1564=ADVANCED_FACE('',(#271),#1489,.T.);
#1565=ADVANCED_FACE('',(#272),#1490,.T.);
#1566=ADVANCED_FACE('',(#273),#1491,.T.);
#1567=ADVANCED_FACE('',(#274),#1492,.F.);
#1568=ADVANCED_FACE('',(#275),#1493,.F.);
#1569=ADVANCED_FACE('',(#276),#1494,.F.);
#1570=ADVANCED_FACE('',(#277,#158),#1495,.F.);
#1571=ADVANCED_FACE('',(#278),#110,.F.);
#1572=ADVANCED_FACE('',(#279),#111,.F.);
#1573=ADVANCED_FACE('',(#280),#1496,.T.);
#1574=ADVANCED_FACE('',(#281),#1497,.T.);
#1575=ADVANCED_FACE('',(#282),#1498,.T.);
#1576=ADVANCED_FACE('',(#283),#1499,.T.);
#1577=ADVANCED_FACE('',(#284,#159),#1500,.T.);
#1578=ADVANCED_FACE('',(#285),#112,.T.);
#1579=ADVANCED_FACE('',(#286),#1501,.T.);
#1580=ADVANCED_FACE('',(#287),#1502,.F.);
#1581=ADVANCED_FACE('',(#288),#113,.F.);
#1582=ADVANCED_FACE('',(#289),#114,.T.);
#1583=ADVANCED_FACE('',(#290,#160),#1503,.T.);
#1584=ADVANCED_FACE('',(#291,#161),#1504,.F.);
#1585=ADVANCED_FACE('',(#292),#59,.T.);
#1586=ADVANCED_FACE('',(#293),#60,.T.);
#1587=ADVANCED_FACE('',(#294),#1505,.T.);
#1588=ADVANCED_FACE('',(#295),#1506,.T.);
#1589=ADVANCED_FACE('',(#296),#1507,.T.);
#1590=ADVANCED_FACE('',(#297),#115,.F.);
#1591=ADVANCED_FACE('',(#298),#1508,.T.);
#1592=ADVANCED_FACE('',(#299),#1509,.T.);
#1593=ADVANCED_FACE('',(#300),#1510,.T.);
#1594=ADVANCED_FACE('',(#301,#162),#1511,.T.);
#1595=ADVANCED_FACE('',(#302,#163),#1512,.F.);
#1596=CLOSED_SHELL('',(#1513,#1514,#1515,#1516,#1517,#1518,#1519,#1520,
#1521,#1522,#1523,#1524,#1525,#1526,#1527,#1528,#1529,#1530,#1531,#1532,
#1533,#1534,#1535,#1536,#1537,#1538,#1539,#1540,#1541,#1542,#1543,#1544,
#1545,#1546));
#1597=CLOSED_SHELL('',(#1547,#1548,#1549,#1550,#1551,#1552,#1553,#1554,
#1555,#1556,#1557));
#1598=CLOSED_SHELL('',(#1558,#1559,#1560,#1561,#1562,#1563,#1564,#1565,
#1566,#1567));
#1599=CLOSED_SHELL('',(#1568,#1569,#1570,#1571,#1572,#1573,#1574,#1575,
#1576,#1577));
#1600=CLOSED_SHELL('',(#1578,#1579,#1580));
#1601=CLOSED_SHELL('',(#1581,#1582,#1583,#1584));
#1602=CLOSED_SHELL('',(#1585,#1586,#1587,#1588,#1589,#1590,#1591,#1592,
#1593,#1594,#1595));
#1603=DERIVED_UNIT_ELEMENT(#1617,1.);
#1604=DERIVED_UNIT_ELEMENT(#2770,-3.);
#1605=DERIVED_UNIT_ELEMENT(#1617,1.);
#1606=DERIVED_UNIT_ELEMENT(#2770,-3.);
#1607=DERIVED_UNIT_ELEMENT(#1617,1.);
#1608=DERIVED_UNIT_ELEMENT(#2770,-3.);
#1609=DERIVED_UNIT_ELEMENT(#1617,1.);
#1610=DERIVED_UNIT_ELEMENT(#2770,-3.);
#1611=DERIVED_UNIT_ELEMENT(#1617,1.);
#1612=DERIVED_UNIT_ELEMENT(#2770,-3.);
#1613=DERIVED_UNIT_ELEMENT(#1617,1.);
#1614=DERIVED_UNIT_ELEMENT(#2770,-3.);
#1615=DERIVED_UNIT_ELEMENT(#1617,1.);
#1616=DERIVED_UNIT_ELEMENT(#2770,-3.);
#1617=(
MASS_UNIT()
NAMED_UNIT(*)
SI_UNIT(.KILO.,.GRAM.)
);
#1618=DERIVED_UNIT((#1603,#1604));
#1619=DERIVED_UNIT((#1605,#1606));
#1620=DERIVED_UNIT((#1607,#1608));
#1621=DERIVED_UNIT((#1609,#1610));
#1622=DERIVED_UNIT((#1611,#1612));
#1623=DERIVED_UNIT((#1613,#1614));
#1624=DERIVED_UNIT((#1615,#1616));
#1625=MEASURE_REPRESENTATION_ITEM('density measure',
POSITIVE_RATIO_MEASURE(7850.),#1618);
#1626=MEASURE_REPRESENTATION_ITEM('density measure',
POSITIVE_RATIO_MEASURE(7850.),#1619);
#1627=MEASURE_REPRESENTATION_ITEM('density measure',
POSITIVE_RATIO_MEASURE(7850.),#1620);
#1628=MEASURE_REPRESENTATION_ITEM('density measure',
POSITIVE_RATIO_MEASURE(7850.),#1621);
#1629=MEASURE_REPRESENTATION_ITEM('density measure',
POSITIVE_RATIO_MEASURE(7850.),#1622);
#1630=MEASURE_REPRESENTATION_ITEM('density measure',
POSITIVE_RATIO_MEASURE(7850.),#1623);
#1631=MEASURE_REPRESENTATION_ITEM('density measure',
POSITIVE_RATIO_MEASURE(7850.),#1624);
#1632=PROPERTY_DEFINITION_REPRESENTATION(#1667,#1646);
#1633=PROPERTY_DEFINITION_REPRESENTATION(#1668,#1647);
#1634=PROPERTY_DEFINITION_REPRESENTATION(#1669,#1648);
#1635=PROPERTY_DEFINITION_REPRESENTATION(#1670,#1649);
#1636=PROPERTY_DEFINITION_REPRESENTATION(#1671,#1650);
#1637=PROPERTY_DEFINITION_REPRESENTATION(#1672,#1651);
#1638=PROPERTY_DEFINITION_REPRESENTATION(#1673,#1652);
#1639=PROPERTY_DEFINITION_REPRESENTATION(#1674,#1653);
#1640=PROPERTY_DEFINITION_REPRESENTATION(#1675,#1654);
#1641=PROPERTY_DEFINITION_REPRESENTATION(#1676,#1655);
#1642=PROPERTY_DEFINITION_REPRESENTATION(#1677,#1656);
#1643=PROPERTY_DEFINITION_REPRESENTATION(#1678,#1657);
#1644=PROPERTY_DEFINITION_REPRESENTATION(#1679,#1658);
#1645=PROPERTY_DEFINITION_REPRESENTATION(#1680,#1659);
#1646=REPRESENTATION('material name',(#1660),#2761);
#1647=REPRESENTATION('density',(#1625),#2761);
#1648=REPRESENTATION('material name',(#1661),#2762);
#1649=REPRESENTATION('density',(#1626),#2762);
#1650=REPRESENTATION('material name',(#1662),#2763);
#1651=REPRESENTATION('density',(#1627),#2763);
#1652=REPRESENTATION('material name',(#1663),#2764);
#1653=REPRESENTATION('density',(#1628),#2764);
#1654=REPRESENTATION('material name',(#1664),#2765);
#1655=REPRESENTATION('density',(#1629),#2765);
#1656=REPRESENTATION('material name',(#1665),#2766);
#1657=REPRESENTATION('density',(#1630),#2766);
#1658=REPRESENTATION('material name',(#1666),#2767);
#1659=REPRESENTATION('density',(#1631),#2767);
#1660=DESCRIPTIVE_REPRESENTATION_ITEM('Steel','Steel');
#1661=DESCRIPTIVE_REPRESENTATION_ITEM('Steel','Steel');
#1662=DESCRIPTIVE_REPRESENTATION_ITEM('Steel','Steel');
#1663=DESCRIPTIVE_REPRESENTATION_ITEM('Steel','Steel');
#1664=DESCRIPTIVE_REPRESENTATION_ITEM('Steel','Steel');
#1665=DESCRIPTIVE_REPRESENTATION_ITEM('Steel','Steel');
#1666=DESCRIPTIVE_REPRESENTATION_ITEM('Steel','Steel');
#1667=PROPERTY_DEFINITION('material property','material name',#2808);
#1668=PROPERTY_DEFINITION('material property','density of part',#2808);
#1669=PROPERTY_DEFINITION('material property','material name',#2809);
#1670=PROPERTY_DEFINITION('material property','density of part',#2809);
#1671=PROPERTY_DEFINITION('material property','material name',#2810);
#1672=PROPERTY_DEFINITION('material property','density of part',#2810);
#1673=PROPERTY_DEFINITION('material property','material name',#2811);
#1674=PROPERTY_DEFINITION('material property','density of part',#2811);
#1675=PROPERTY_DEFINITION('material property','material name',#2812);
#1676=PROPERTY_DEFINITION('material property','density of part',#2812);
#1677=PROPERTY_DEFINITION('material property','material name',#2813);
#1678=PROPERTY_DEFINITION('material property','density of part',#2813);
#1679=PROPERTY_DEFINITION('material property','material name',#2814);
#1680=PROPERTY_DEFINITION('material property','density of part',#2814);
#1681=AXIS2_PLACEMENT_3D('',#2286,#1837,#1838);
#1682=AXIS2_PLACEMENT_3D('',#2287,#1839,#1840);
#1683=AXIS2_PLACEMENT_3D('',#2288,#1841,#1842);
#1684=AXIS2_PLACEMENT_3D('',#2297,#1847,#1848);
#1685=AXIS2_PLACEMENT_3D('',#2303,#1852,#1853);
#1686=AXIS2_PLACEMENT_3D('',#2312,#1858,#1859);
#1687=AXIS2_PLACEMENT_3D('',#2318,#1863,#1864);
#1688=AXIS2_PLACEMENT_3D('',#2324,#1868,#1869);
#1689=AXIS2_PLACEMENT_3D('',#2330,#1873,#1874);
#1690=AXIS2_PLACEMENT_3D('',#2333,#1877,#1878);
#1691=AXIS2_PLACEMENT_3D('',#2343,#1884,#1885);
#1692=AXIS2_PLACEMENT_3D('',#2348,#1888,#1889);
#1693=AXIS2_PLACEMENT_3D('',#2350,#1890,#1891);
#1694=AXIS2_PLACEMENT_3D('',#2352,#1892,#1893);
#1695=AXIS2_PLACEMENT_3D('',#2354,#1894,#1895);
#1696=AXIS2_PLACEMENT_3D('',#2356,#1896,#1897);
#1697=AXIS2_PLACEMENT_3D('',#2358,#1898,#1899);
#1698=AXIS2_PLACEMENT_3D('',#2360,#1900,#1901);
#1699=AXIS2_PLACEMENT_3D('',#2362,#1902,#1903);
#1700=AXIS2_PLACEMENT_3D('',#2364,#1904,#1905);
#1701=AXIS2_PLACEMENT_3D('',#2366,#1906,#1907);
#1702=AXIS2_PLACEMENT_3D('',#2367,#1908,#1909);
#1703=AXIS2_PLACEMENT_3D('',#2372,#1912,#1913);
#1704=AXIS2_PLACEMENT_3D('',#2374,#1914,#1915);
#1705=AXIS2_PLACEMENT_3D('',#2376,#1916,#1917);
#1706=AXIS2_PLACEMENT_3D('',#2378,#1918,#1919);
#1707=AXIS2_PLACEMENT_3D('',#2380,#1920,#1921);
#1708=AXIS2_PLACEMENT_3D('',#2382,#1922,#1923);
#1709=AXIS2_PLACEMENT_3D('',#2384,#1924,#1925);
#1710=AXIS2_PLACEMENT_3D('',#2386,#1926,#1927);
#1711=AXIS2_PLACEMENT_3D('',#2388,#1928,#1929);
#1712=AXIS2_PLACEMENT_3D('',#2390,#1930,#1931);
#1713=AXIS2_PLACEMENT_3D('',#2391,#1932,#1933);
#1714=AXIS2_PLACEMENT_3D('',#2393,#1934,#1935);
#1715=AXIS2_PLACEMENT_3D('',#2395,#1937,#1938);
#1716=AXIS2_PLACEMENT_3D('',#2397,#1939,#1940);
#1717=AXIS2_PLACEMENT_3D('',#2399,#1942,#1943);
#1718=AXIS2_PLACEMENT_3D('',#2401,#1944,#1945);
#1719=AXIS2_PLACEMENT_3D('',#2403,#1947,#1948);
#1720=AXIS2_PLACEMENT_3D('',#2405,#1949,#1950);
#1721=AXIS2_PLACEMENT_3D('',#2407,#1952,#1953);
#1722=AXIS2_PLACEMENT_3D('',#2409,#1954,#1955);
#1723=AXIS2_PLACEMENT_3D('',#2411,#1957,#1958);
#1724=AXIS2_PLACEMENT_3D('',#2413,#1959,#1960);
#1725=AXIS2_PLACEMENT_3D('',#2415,#1962,#1963);
#1726=AXIS2_PLACEMENT_3D('',#2417,#1964,#1965);
#1727=AXIS2_PLACEMENT_3D('',#2419,#1967,#1968);
#1728=AXIS2_PLACEMENT_3D('',#2421,#1969,#1970);
#1729=AXIS2_PLACEMENT_3D('',#2423,#1972,#1973);
#1730=AXIS2_PLACEMENT_3D('',#2425,#1974,#1975);
#1731=AXIS2_PLACEMENT_3D('',#2427,#1977,#1978);
#1732=AXIS2_PLACEMENT_3D('',#2429,#1979,#1980);
#1733=AXIS2_PLACEMENT_3D('',#2431,#1982,#1983);
#1734=AXIS2_PLACEMENT_3D('',#2433,#1984,#1985);
#1735=AXIS2_PLACEMENT_3D('',#2435,#1987,#1988);
#1736=AXIS2_PLACEMENT_3D('',#2437,#1989,#1990);
#1737=AXIS2_PLACEMENT_3D('',#2439,#1992,#1993);
#1738=AXIS2_PLACEMENT_3D('',#2441,#1994,#1995);
#1739=AXIS2_PLACEMENT_3D('',#2443,#1997,#1998);
#1740=AXIS2_PLACEMENT_3D('',#2445,#1999,#2000);
#1741=AXIS2_PLACEMENT_3D('',#2447,#2002,#2003);
#1742=AXIS2_PLACEMENT_3D('',#2449,#2004,#2005);
#1743=AXIS2_PLACEMENT_3D('',#2451,#2007,#2008);
#1744=AXIS2_PLACEMENT_3D('',#2453,#2009,#2010);
#1745=AXIS2_PLACEMENT_3D('',#2455,#2012,#2013);
#1746=AXIS2_PLACEMENT_3D('',#2457,#2014,#2015);
#1747=AXIS2_PLACEMENT_3D('',#2459,#2017,#2018);
#1748=AXIS2_PLACEMENT_3D('',#2461,#2019,#2020);
#1749=AXIS2_PLACEMENT_3D('',#2463,#2022,#2023);
#1750=AXIS2_PLACEMENT_3D('',#2465,#2024,#2025);
#1751=AXIS2_PLACEMENT_3D('',#2467,#2027,#2028);
#1752=AXIS2_PLACEMENT_3D('',#2469,#2029,#2030);
#1753=AXIS2_PLACEMENT_3D('',#2471,#2032,#2033);
#1754=AXIS2_PLACEMENT_3D('',#2475,#2036,#2037);
#1755=AXIS2_PLACEMENT_3D('',#2479,#2040,#2041);
#1756=AXIS2_PLACEMENT_3D('',#2481,#2043,#2044);
#1757=AXIS2_PLACEMENT_3D('',#2482,#2045,#2046);
#1758=AXIS2_PLACEMENT_3D('',#2483,#2047,#2048);
#1759=AXIS2_PLACEMENT_3D('',#2485,#2049,#2050);
#1760=AXIS2_PLACEMENT_3D('',#2488,#2052,#2053);
#1761=AXIS2_PLACEMENT_3D('',#2489,#2054,#2055);
#1762=AXIS2_PLACEMENT_3D('',#2498,#2060,#2061);
#1763=AXIS2_PLACEMENT_3D('',#2507,#2066,#2067);
#1764=AXIS2_PLACEMENT_3D('',#2510,#2070,#2071);
#1765=AXIS2_PLACEMENT_3D('',#2516,#2075,#2076);
#1766=AXIS2_PLACEMENT_3D('',#2522,#2080,#2081);
#1767=AXIS2_PLACEMENT_3D('',#2528,#2085,#2086);
#1768=AXIS2_PLACEMENT_3D('',#2532,#2089,#2090);
#1769=AXIS2_PLACEMENT_3D('',#2536,#2093,#2094);
#1770=AXIS2_PLACEMENT_3D('',#2538,#2096,#2097);
#1771=AXIS2_PLACEMENT_3D('',#2539,#2098,#2099);
#1772=AXIS2_PLACEMENT_3D('',#2540,#2100,#2101);
#1773=AXIS2_PLACEMENT_3D('',#2549,#2106,#2107);
#1774=AXIS2_PLACEMENT_3D('',#2555,#2111,#2112);
#1775=AXIS2_PLACEMENT_3D('',#2561,#2116,#2117);
#1776=AXIS2_PLACEMENT_3D('',#2567,#2121,#2122);
#1777=AXIS2_PLACEMENT_3D('',#2573,#2126,#2127);
#1778=AXIS2_PLACEMENT_3D('',#2579,#2131,#2132);
#1779=AXIS2_PLACEMENT_3D('',#2585,#2136,#2137);
#1780=AXIS2_PLACEMENT_3D('',#2588,#2140,#2141);
#1781=AXIS2_PLACEMENT_3D('',#2589,#2142,#2143);
#1782=AXIS2_PLACEMENT_3D('',#2590,#2144,#2145);
#1783=AXIS2_PLACEMENT_3D('',#2591,#2146,#2147);
#1784=AXIS2_PLACEMENT_3D('',#2600,#2152,#2153);
#1785=AXIS2_PLACEMENT_3D('',#2609,#2158,#2159);
#1786=AXIS2_PLACEMENT_3D('',#2618,#2164,#2165);
#1787=AXIS2_PLACEMENT_3D('',#2619,#2166,#2167);
#1788=AXIS2_PLACEMENT_3D('',#2620,#2168,#2169);
#1789=AXIS2_PLACEMENT_3D('',#2621,#2170,#2171);
#1790=AXIS2_PLACEMENT_3D('',#2622,#2172,#2173);
#1791=AXIS2_PLACEMENT_3D('',#2623,#2174,#2175);
#1792=AXIS2_PLACEMENT_3D('',#2624,#2176,#2177);
#1793=AXIS2_PLACEMENT_3D('',#2630,#2181,#2182);
#1794=AXIS2_PLACEMENT_3D('',#2634,#2185,#2186);
#1795=AXIS2_PLACEMENT_3D('',#2638,#2189,#2190);
#1796=AXIS2_PLACEMENT_3D('',#2640,#2192,#2193);
#1797=AXIS2_PLACEMENT_3D('',#2641,#2194,#2195);
#1798=AXIS2_PLACEMENT_3D('',#2642,#2196,#2197);
#1799=AXIS2_PLACEMENT_3D('',#2644,#2198,#2199);
#1800=AXIS2_PLACEMENT_3D('',#2647,#2201,#2202);
#1801=AXIS2_PLACEMENT_3D('',#2648,#2203,#2204);
#1802=AXIS2_PLACEMENT_3D('',#2649,#2205,#2206);
#1803=AXIS2_PLACEMENT_3D('',#2650,#2207,#2208);
#1804=AXIS2_PLACEMENT_3D('',#2651,#2209,#2210);
#1805=AXIS2_PLACEMENT_3D('',#2653,#2211,#2212);
#1806=AXIS2_PLACEMENT_3D('',#2656,#2214,#2215);
#1807=AXIS2_PLACEMENT_3D('',#2657,#2216,#2217);
#1808=AXIS2_PLACEMENT_3D('',#2659,#2218,#2219);
#1809=AXIS2_PLACEMENT_3D('',#2662,#2221,#2222);
#1810=AXIS2_PLACEMENT_3D('',#2663,#2223,#2224);
#1811=AXIS2_PLACEMENT_3D('',#2664,#2225,#2226);
#1812=AXIS2_PLACEMENT_3D('',#2665,#2227,#2228);
#1813=AXIS2_PLACEMENT_3D('',#2666,#2229,#2230);
#1814=AXIS2_PLACEMENT_3D('',#2678,#2232,#2233);
#1815=AXIS2_PLACEMENT_3D('',#2694,#2234,#2235);
#1816=AXIS2_PLACEMENT_3D('',#2696,#2236,#2237);
#1817=AXIS2_PLACEMENT_3D('',#2722,#2239,#2240);
#1818=AXIS2_PLACEMENT_3D('',#2725,#2243,#2244);
#1819=AXIS2_PLACEMENT_3D('',#2727,#2246,#2247);
#1820=AXIS2_PLACEMENT_3D('',#2729,#2249,#2250);
#1821=AXIS2_PLACEMENT_3D('',#2731,#2251,#2252);
#1822=AXIS2_PLACEMENT_3D('',#2734,#2254,#2255);
#1823=AXIS2_PLACEMENT_3D('',#2735,#2256,#2257);
#1824=AXIS2_PLACEMENT_3D('',#2737,#2259,#2260);
#1825=AXIS2_PLACEMENT_3D('',#2739,#2262,#2263);
#1826=AXIS2_PLACEMENT_3D('',#2740,#2264,#2265);
#1827=AXIS2_PLACEMENT_3D('',#2741,#2266,#2267);
#1828=AXIS2_PLACEMENT_3D('',#2742,#2268,#2269);
#1829=AXIS2_PLACEMENT_3D('',#2743,#2270,#2271);
#1830=AXIS2_PLACEMENT_3D('',#2744,#2272,#2273);
#1831=AXIS2_PLACEMENT_3D('',#2745,#2274,#2275);
#1832=AXIS2_PLACEMENT_3D('',#2746,#2276,#2277);
#1833=AXIS2_PLACEMENT_3D('',#2747,#2278,#2279);
#1834=AXIS2_PLACEMENT_3D('',#2748,#2280,#2281);
#1835=AXIS2_PLACEMENT_3D('',#2749,#2282,#2283);
#1836=AXIS2_PLACEMENT_3D('',#2750,#2284,#2285);
#1837=DIRECTION('axis',(0.,0.,1.));
#1838=DIRECTION('refdir',(1.,0.,0.));
#1839=DIRECTION('axis',(0.,0.,1.));
#1840=DIRECTION('refdir',(1.,0.,0.));
#1841=DIRECTION('center_axis',(0.,-1.,0.));
#1842=DIRECTION('ref_axis',(0.,0.,-1.));
#1843=DIRECTION('',(0.,0.,1.));
#1844=DIRECTION('',(1.,0.,0.));
#1845=DIRECTION('',(0.,0.,-1.));
#1846=DIRECTION('',(-1.,0.,0.));
#1847=DIRECTION('center_axis',(0.,0.,1.));
#1848=DIRECTION('ref_axis',(0.,-1.,0.));
#1849=DIRECTION('',(0.,1.,0.));
#1850=DIRECTION('',(1.,0.,0.));
#1851=DIRECTION('',(0.,-1.,0.));
#1852=DIRECTION('center_axis',(0.,1.,0.));
#1853=DIRECTION('ref_axis',(0.,0.,1.));
#1854=DIRECTION('',(0.,0.,-1.));
#1855=DIRECTION('',(1.,0.,0.));
#1856=DIRECTION('',(0.,0.,1.));
#1857=DIRECTION('',(1.,0.,0.));
#1858=DIRECTION('center_axis',(0.,0.,1.));
#1859=DIRECTION('ref_axis',(0.,-1.,0.));
#1860=DIRECTION('',(0.,1.,0.));
#1861=DIRECTION('',(0.,-1.,0.));
#1862=DIRECTION('',(1.,0.,0.));
#1863=DIRECTION('center_axis',(0.,1.,0.));
#1864=DIRECTION('ref_axis',(0.,0.,1.));
#1865=DIRECTION('',(0.,0.,-1.));
#1866=DIRECTION('',(0.,0.,1.));
#1867=DIRECTION('',(1.,0.,0.));
#1868=DIRECTION('center_axis',(0.,0.,-1.));
#1869=DIRECTION('ref_axis',(0.,1.,0.));
#1870=DIRECTION('',(0.,-1.,0.));
#1871=DIRECTION('',(0.,1.,0.));
#1872=DIRECTION('',(1.,0.,0.));
#1873=DIRECTION('center_axis',(0.,-1.,0.));
#1874=DIRECTION('ref_axis',(0.,0.,-1.));
#1875=DIRECTION('',(0.,0.,1.));
#1876=DIRECTION('',(0.,0.,-1.));
#1877=DIRECTION('center_axis',(-1.,0.,0.));
#1878=DIRECTION('ref_axis',(0.,-1.,0.));
#1879=DIRECTION('',(0.,-1.,0.));
#1880=DIRECTION('',(0.,0.,1.));
#1881=DIRECTION('',(0.,-1.,0.));
#1882=DIRECTION('',(0.,0.,1.));
#1883=DIRECTION('',(0.,-1.,0.));
#1884=DIRECTION('center_axis',(0.,0.,1.));
#1885=DIRECTION('ref_axis',(1.,0.,0.));
#1886=DIRECTION('',(0.,1.,0.));
#1887=DIRECTION('',(-1.,0.,0.));
#1888=DIRECTION('center_axis',(0.,0.,-1.));
#1889=DIRECTION('ref_axis',(1.,0.,0.));
#1890=DIRECTION('center_axis',(0.,0.,-1.));
#1891=DIRECTION('ref_axis',(1.,0.,0.));
#1892=DIRECTION('center_axis',(0.,0.,-1.));
#1893=DIRECTION('ref_axis',(1.,0.,0.));
#1894=DIRECTION('center_axis',(0.,0.,-1.));
#1895=DIRECTION('ref_axis',(1.,0.,0.));
#1896=DIRECTION('center_axis',(0.,0.,-1.));
#1897=DIRECTION('ref_axis',(1.,0.,0.));
#1898=DIRECTION('center_axis',(0.,0.,-1.));
#1899=DIRECTION('ref_axis',(1.,0.,0.));
#1900=DIRECTION('center_axis',(0.,0.,-1.));
#1901=DIRECTION('ref_axis',(1.,0.,0.));
#1902=DIRECTION('center_axis',(0.,0.,-1.));
#1903=DIRECTION('ref_axis',(1.,0.,0.));
#1904=DIRECTION('center_axis',(0.,0.,-1.));
#1905=DIRECTION('ref_axis',(1.,0.,0.));
#1906=DIRECTION('center_axis',(0.,0.,-1.));
#1907=DIRECTION('ref_axis',(1.,0.,0.));
#1908=DIRECTION('center_axis',(0.,0.,1.));
#1909=DIRECTION('ref_axis',(1.,0.,0.));
#1910=DIRECTION('',(1.,0.,0.));
#1911=DIRECTION('',(0.,1.,0.));
#1912=DIRECTION('center_axis',(0.,0.,-1.));
#1913=DIRECTION('ref_axis',(1.,0.,0.));
#1914=DIRECTION('center_axis',(0.,0.,-1.));
#1915=DIRECTION('ref_axis',(1.,0.,0.));
#1916=DIRECTION('center_axis',(0.,0.,-1.));
#1917=DIRECTION('ref_axis',(1.,0.,0.));
#1918=DIRECTION('center_axis',(0.,0.,-1.));
#1919=DIRECTION('ref_axis',(1.,0.,0.));
#1920=DIRECTION('center_axis',(0.,0.,-1.));
#1921=DIRECTION('ref_axis',(1.,0.,0.));
#1922=DIRECTION('center_axis',(0.,0.,-1.));
#1923=DIRECTION('ref_axis',(1.,0.,0.));
#1924=DIRECTION('center_axis',(0.,0.,-1.));
#1925=DIRECTION('ref_axis',(1.,0.,0.));
#1926=DIRECTION('center_axis',(0.,0.,-1.));
#1927=DIRECTION('ref_axis',(1.,0.,0.));
#1928=DIRECTION('center_axis',(0.,0.,-1.));
#1929=DIRECTION('ref_axis',(1.,0.,0.));
#1930=DIRECTION('center_axis',(0.,0.,-1.));
#1931=DIRECTION('ref_axis',(1.,0.,0.));
#1932=DIRECTION('center_axis',(0.,0.,1.));
#1933=DIRECTION('ref_axis',(1.,0.,0.));
#1934=DIRECTION('center_axis',(0.,0.,1.));
#1935=DIRECTION('ref_axis',(1.,0.,0.));
#1936=DIRECTION('',(0.,0.,1.));
#1937=DIRECTION('center_axis',(0.,0.,1.));
#1938=DIRECTION('ref_axis',(1.,0.,0.));
#1939=DIRECTION('center_axis',(0.,0.,1.));
#1940=DIRECTION('ref_axis',(1.,0.,0.));
#1941=DIRECTION('',(0.,0.,1.));
#1942=DIRECTION('center_axis',(0.,0.,1.));
#1943=DIRECTION('ref_axis',(1.,0.,0.));
#1944=DIRECTION('center_axis',(0.,0.,1.));
#1945=DIRECTION('ref_axis',(1.,0.,0.));
#1946=DIRECTION('',(0.,0.,1.));
#1947=DIRECTION('center_axis',(0.,0.,1.));
#1948=DIRECTION('ref_axis',(1.,0.,0.));
#1949=DIRECTION('center_axis',(0.,0.,1.));
#1950=DIRECTION('ref_axis',(1.,0.,0.));
#1951=DIRECTION('',(0.,0.,1.));
#1952=DIRECTION('center_axis',(0.,0.,1.));
#1953=DIRECTION('ref_axis',(1.,0.,0.));
#1954=DIRECTION('center_axis',(0.,0.,1.));
#1955=DIRECTION('ref_axis',(1.,0.,0.));
#1956=DIRECTION('',(0.,0.,1.));
#1957=DIRECTION('center_axis',(0.,0.,1.));
#1958=DIRECTION('ref_axis',(1.,0.,0.));
#1959=DIRECTION('center_axis',(0.,0.,1.));
#1960=DIRECTION('ref_axis',(1.,0.,0.));
#1961=DIRECTION('',(0.,0.,1.));
#1962=DIRECTION('center_axis',(0.,0.,1.));
#1963=DIRECTION('ref_axis',(1.,0.,0.));
#1964=DIRECTION('center_axis',(0.,0.,1.));
#1965=DIRECTION('ref_axis',(1.,0.,0.));
#1966=DIRECTION('',(0.,0.,1.));
#1967=DIRECTION('center_axis',(0.,0.,1.));
#1968=DIRECTION('ref_axis',(1.,0.,0.));
#1969=DIRECTION('center_axis',(0.,0.,1.));
#1970=DIRECTION('ref_axis',(1.,0.,0.));
#1971=DIRECTION('',(0.,0.,1.));
#1972=DIRECTION('center_axis',(0.,0.,1.));
#1973=DIRECTION('ref_axis',(1.,0.,0.));
#1974=DIRECTION('center_axis',(0.,0.,1.));
#1975=DIRECTION('ref_axis',(1.,0.,0.));
#1976=DIRECTION('',(0.,0.,1.));
#1977=DIRECTION('center_axis',(0.,0.,1.));
#1978=DIRECTION('ref_axis',(1.,0.,0.));
#1979=DIRECTION('center_axis',(0.,0.,1.));
#1980=DIRECTION('ref_axis',(1.,0.,0.));
#1981=DIRECTION('',(0.,0.,1.));
#1982=DIRECTION('center_axis',(0.,0.,1.));
#1983=DIRECTION('ref_axis',(1.,0.,0.));
#1984=DIRECTION('center_axis',(0.,0.,1.));
#1985=DIRECTION('ref_axis',(1.,0.,0.));
#1986=DIRECTION('',(0.,0.,1.));
#1987=DIRECTION('center_axis',(0.,0.,1.));
#1988=DIRECTION('ref_axis',(1.,0.,0.));
#1989=DIRECTION('center_axis',(0.,0.,1.));
#1990=DIRECTION('ref_axis',(1.,0.,0.));
#1991=DIRECTION('',(0.,0.,1.));
#1992=DIRECTION('center_axis',(0.,0.,1.));
#1993=DIRECTION('ref_axis',(1.,0.,0.));
#1994=DIRECTION('center_axis',(0.,0.,1.));
#1995=DIRECTION('ref_axis',(1.,0.,0.));
#1996=DIRECTION('',(0.,0.,1.));
#1997=DIRECTION('center_axis',(0.,0.,1.));
#1998=DIRECTION('ref_axis',(1.,0.,0.));
#1999=DIRECTION('center_axis',(0.,0.,1.));
#2000=DIRECTION('ref_axis',(1.,0.,0.));
#2001=DIRECTION('',(0.,0.,1.));
#2002=DIRECTION('center_axis',(0.,0.,1.));
#2003=DIRECTION('ref_axis',(1.,0.,0.));
#2004=DIRECTION('center_axis',(0.,0.,1.));
#2005=DIRECTION('ref_axis',(1.,0.,0.));
#2006=DIRECTION('',(0.,0.,1.));
#2007=DIRECTION('center_axis',(0.,0.,1.));
#2008=DIRECTION('ref_axis',(1.,0.,0.));
#2009=DIRECTION('center_axis',(0.,0.,1.));
#2010=DIRECTION('ref_axis',(1.,0.,0.));
#2011=DIRECTION('',(0.,0.,1.));
#2012=DIRECTION('center_axis',(0.,0.,1.));
#2013=DIRECTION('ref_axis',(1.,0.,0.));
#2014=DIRECTION('center_axis',(0.,0.,1.));
#2015=DIRECTION('ref_axis',(1.,0.,0.));
#2016=DIRECTION('',(0.,0.,1.));
#2017=DIRECTION('center_axis',(0.,0.,1.));
#2018=DIRECTION('ref_axis',(1.,0.,0.));
#2019=DIRECTION('center_axis',(0.,0.,1.));
#2020=DIRECTION('ref_axis',(1.,0.,0.));
#2021=DIRECTION('',(0.,0.,1.));
#2022=DIRECTION('center_axis',(0.,0.,1.));
#2023=DIRECTION('ref_axis',(1.,0.,0.));
#2024=DIRECTION('center_axis',(0.,0.,1.));
#2025=DIRECTION('ref_axis',(1.,0.,0.));
#2026=DIRECTION('',(0.,0.,1.));
#2027=DIRECTION('center_axis',(0.,0.,1.));
#2028=DIRECTION('ref_axis',(1.,0.,0.));
#2029=DIRECTION('center_axis',(0.,0.,1.));
#2030=DIRECTION('ref_axis',(1.,0.,0.));
#2031=DIRECTION('',(0.,0.,1.));
#2032=DIRECTION('center_axis',(0.,1.,0.));
#2033=DIRECTION('ref_axis',(-1.,0.,0.));
#2034=DIRECTION('',(-1.,0.,0.));
#2035=DIRECTION('',(0.,0.,1.));
#2036=DIRECTION('center_axis',(1.,0.,0.));
#2037=DIRECTION('ref_axis',(0.,1.,0.));
#2038=DIRECTION('',(0.,0.,1.));
#2039=DIRECTION('',(0.,1.,0.));
#2040=DIRECTION('center_axis',(0.,-1.,0.));
#2041=DIRECTION('ref_axis',(1.,0.,0.));
#2042=DIRECTION('',(1.,0.,0.));
#2043=DIRECTION('center_axis',(0.,0.,1.));
#2044=DIRECTION('ref_axis',(1.,0.,0.));
#2045=DIRECTION('axis',(0.,0.,1.));
#2046=DIRECTION('refdir',(1.,0.,0.));
#2047=DIRECTION('center_axis',(0.,0.,1.));
#2048=DIRECTION('ref_axis',(1.,0.,0.));
#2049=DIRECTION('center_axis',(0.,0.,1.));
#2050=DIRECTION('ref_axis',(1.,0.,0.));
#2051=DIRECTION('',(0.,0.,1.));
#2052=DIRECTION('center_axis',(0.,0.,-1.));
#2053=DIRECTION('ref_axis',(1.,0.,0.));
#2054=DIRECTION('center_axis',(0.,1.,0.));
#2055=DIRECTION('ref_axis',(-1.,0.,0.));
#2056=DIRECTION('',(1.,0.,0.));
#2057=DIRECTION('',(0.,0.,1.));
#2058=DIRECTION('',(-1.,0.,0.));
#2059=DIRECTION('',(0.,0.,1.));
#2060=DIRECTION('center_axis',(0.,-1.,0.));
#2061=DIRECTION('ref_axis',(1.,0.,0.));
#2062=DIRECTION('',(-1.,0.,0.));
#2063=DIRECTION('',(0.,0.,1.));
#2064=DIRECTION('',(1.,0.,0.));
#2065=DIRECTION('',(0.,0.,1.));
#2066=DIRECTION('center_axis',(0.,0.,1.));
#2067=DIRECTION('ref_axis',(1.,0.,0.));
#2068=DIRECTION('',(0.,-1.,0.));
#2069=DIRECTION('',(0.,1.,0.));
#2070=DIRECTION('center_axis',(0.,0.,1.));
#2071=DIRECTION('ref_axis',(1.,0.,0.));
#2072=DIRECTION('',(0.,1.,0.));
#2073=DIRECTION('',(-1.,0.,0.));
#2074=DIRECTION('',(0.,-1.,0.));
#2075=DIRECTION('center_axis',(0.,0.,1.));
#2076=DIRECTION('ref_axis',(1.,0.,0.));
#2077=DIRECTION('',(0.,-1.,0.));
#2078=DIRECTION('',(1.,0.,0.));
#2079=DIRECTION('',(0.,1.,0.));
#2080=DIRECTION('center_axis',(0.,1.,0.));
#2081=DIRECTION('ref_axis',(-1.,0.,0.));
#2082=DIRECTION('',(-1.,0.,0.));
#2083=DIRECTION('',(0.,0.,1.));
#2084=DIRECTION('',(0.,0.,1.));
#2085=DIRECTION('center_axis',(1.,0.,0.));
#2086=DIRECTION('ref_axis',(0.,1.,0.));
#2087=DIRECTION('',(0.,1.,0.));
#2088=DIRECTION('',(0.,0.,1.));
#2089=DIRECTION('center_axis',(0.,-1.,0.));
#2090=DIRECTION('ref_axis',(1.,0.,0.));
#2091=DIRECTION('',(1.,0.,0.));
#2092=DIRECTION('',(0.,0.,1.));
#2093=DIRECTION('center_axis',(-1.,0.,0.));
#2094=DIRECTION('ref_axis',(0.,-1.,0.));
#2095=DIRECTION('',(0.,-1.,0.));
#2096=DIRECTION('center_axis',(0.,0.,1.));
#2097=DIRECTION('ref_axis',(1.,0.,0.));
#2098=DIRECTION('axis',(0.,0.,1.));
#2099=DIRECTION('refdir',(1.,0.,0.));
#2100=DIRECTION('center_axis',(-1.,0.,0.));
#2101=DIRECTION('ref_axis',(0.,0.,1.));
#2102=DIRECTION('',(0.,0.,-1.));
#2103=DIRECTION('',(0.,1.,0.));
#2104=DIRECTION('',(0.,0.,1.));
#2105=DIRECTION('',(0.,1.,0.));
#2106=DIRECTION('center_axis',(0.,0.,-1.));
#2107=DIRECTION('ref_axis',(-1.,0.,0.));
#2108=DIRECTION('',(1.,0.,0.));
#2109=DIRECTION('',(-1.,0.,0.));
#2110=DIRECTION('',(0.,1.,0.));
#2111=DIRECTION('center_axis',(1.,0.,0.));
#2112=DIRECTION('ref_axis',(0.,0.,-1.));
#2113=DIRECTION('',(0.,0.,1.));
#2114=DIRECTION('',(0.,0.,-1.));
#2115=DIRECTION('',(0.,1.,0.));
#2116=DIRECTION('center_axis',(0.,0.,1.));
#2117=DIRECTION('ref_axis',(1.,0.,0.));
#2118=DIRECTION('',(-1.,0.,0.));
#2119=DIRECTION('',(1.,0.,0.));
#2120=DIRECTION('',(0.,1.,0.));
#2121=DIRECTION('center_axis',(-1.,0.,0.));
#2122=DIRECTION('ref_axis',(0.,0.,1.));
#2123=DIRECTION('',(0.,0.,-1.));
#2124=DIRECTION('',(0.,0.,1.));
#2125=DIRECTION('',(0.,1.,0.));
#2126=DIRECTION('center_axis',(0.,0.,1.));
#2127=DIRECTION('ref_axis',(1.,0.,0.));
#2128=DIRECTION('',(-1.,0.,0.));
#2129=DIRECTION('',(1.,0.,0.));
#2130=DIRECTION('',(0.,1.,0.));
#2131=DIRECTION('center_axis',(-1.,0.,0.));
#2132=DIRECTION('ref_axis',(0.,0.,1.));
#2133=DIRECTION('',(0.,0.,-1.));
#2134=DIRECTION('',(0.,0.,1.));
#2135=DIRECTION('',(0.,1.,0.));
#2136=DIRECTION('center_axis',(0.,0.,1.));
#2137=DIRECTION('ref_axis',(1.,0.,0.));
#2138=DIRECTION('',(-1.,0.,0.));
#2139=DIRECTION('',(1.,0.,0.));
#2140=DIRECTION('center_axis',(0.,1.,0.));
#2141=DIRECTION('ref_axis',(0.,0.,1.));
#2142=DIRECTION('center_axis',(0.,1.,0.));
#2143=DIRECTION('ref_axis',(1.,0.,0.));
#2144=DIRECTION('axis',(0.,0.,1.));
#2145=DIRECTION('refdir',(1.,0.,0.));
#2146=DIRECTION('center_axis',(0.,1.,0.));
#2147=DIRECTION('ref_axis',(-1.,0.,0.));
#2148=DIRECTION('',(-1.,0.,0.));
#2149=DIRECTION('',(0.,0.,-1.));
#2150=DIRECTION('',(1.,0.,0.));
#2151=DIRECTION('',(0.,0.,-1.));
#2152=DIRECTION('center_axis',(0.,-1.,0.));
#2153=DIRECTION('ref_axis',(1.,0.,0.));
#2154=DIRECTION('',(1.,0.,0.));
#2155=DIRECTION('',(0.,0.,-1.));
#2156=DIRECTION('',(-1.,0.,0.));
#2157=DIRECTION('',(0.,0.,1.));
#2158=DIRECTION('center_axis',(0.,0.,1.));
#2159=DIRECTION('ref_axis',(1.,0.,0.));
#2160=DIRECTION('',(0.,-1.,0.));
#2161=DIRECTION('',(-1.,0.,0.));
#2162=DIRECTION('',(0.,1.,0.));
#2163=DIRECTION('',(1.,0.,0.));
#2164=DIRECTION('center_axis',(0.,0.,1.));
#2165=DIRECTION('ref_axis',(1.,0.,0.));
#2166=DIRECTION('center_axis',(0.,0.,1.));
#2167=DIRECTION('ref_axis',(1.,0.,0.));
#2168=DIRECTION('center_axis',(0.,0.,1.));
#2169=DIRECTION('ref_axis',(-1.,1.22464679914735E-16,0.));
#2170=DIRECTION('center_axis',(0.,0.,-1.));
#2171=DIRECTION('ref_axis',(1.,0.,0.));
#2172=DIRECTION('center_axis',(0.,0.,1.));
#2173=DIRECTION('ref_axis',(1.,0.,0.));
#2174=DIRECTION('center_axis',(0.,0.,-1.));
#2175=DIRECTION('ref_axis',(1.,0.,0.));
#2176=DIRECTION('center_axis',(0.,1.,0.));
#2177=DIRECTION('ref_axis',(-1.,0.,0.));
#2178=DIRECTION('',(0.,0.,1.));
#2179=DIRECTION('',(-1.,0.,0.));
#2180=DIRECTION('',(0.,0.,1.));
#2181=DIRECTION('center_axis',(1.,0.,0.));
#2182=DIRECTION('ref_axis',(0.,1.,0.));
#2183=DIRECTION('',(0.,1.,0.));
#2184=DIRECTION('',(0.,0.,1.));
#2185=DIRECTION('center_axis',(0.,-1.,0.));
#2186=DIRECTION('ref_axis',(1.,0.,0.));
#2187=DIRECTION('',(1.,0.,0.));
#2188=DIRECTION('',(0.,0.,1.));
#2189=DIRECTION('center_axis',(-1.,0.,0.));
#2190=DIRECTION('ref_axis',(0.,-1.,0.));
#2191=DIRECTION('',(0.,-1.,0.));
#2192=DIRECTION('center_axis',(0.,0.,1.));
#2193=DIRECTION('ref_axis',(1.,0.,0.));
#2194=DIRECTION('axis',(0.,0.,1.));
#2195=DIRECTION('refdir',(1.,0.,0.));
#2196=DIRECTION('center_axis',(0.,0.,1.));
#2197=DIRECTION('ref_axis',(1.,0.,0.));
#2198=DIRECTION('center_axis',(0.,0.,-1.));
#2199=DIRECTION('ref_axis',(1.,0.,0.));
#2200=DIRECTION('',(0.,0.,-1.));
#2201=DIRECTION('center_axis',(0.,0.,-1.));
#2202=DIRECTION('ref_axis',(1.,0.,0.));
#2203=DIRECTION('center_axis',(0.,0.,1.));
#2204=DIRECTION('ref_axis',(1.,0.,0.));
#2205=DIRECTION('center_axis',(0.,0.,1.));
#2206=DIRECTION('ref_axis',(1.,0.,0.));
#2207=DIRECTION('axis',(0.,0.,1.));
#2208=DIRECTION('refdir',(1.,0.,0.));
#2209=DIRECTION('center_axis',(0.,1.,0.));
#2210=DIRECTION('ref_axis',(1.,0.,0.));
#2211=DIRECTION('center_axis',(0.,-1.,0.));
#2212=DIRECTION('ref_axis',(1.,0.,0.));
#2213=DIRECTION('',(0.,-1.,0.));
#2214=DIRECTION('center_axis',(0.,-1.,0.));
#2215=DIRECTION('ref_axis',(1.,0.,0.));
#2216=DIRECTION('center_axis',(0.,1.,0.));
#2217=DIRECTION('ref_axis',(1.,0.,0.));
#2218=DIRECTION('center_axis',(0.,1.,0.));
#2219=DIRECTION('ref_axis',(1.,0.,0.));
#2220=DIRECTION('',(0.,-1.,0.));
#2221=DIRECTION('center_axis',(0.,1.,0.));
#2222=DIRECTION('ref_axis',(1.,0.,0.));
#2223=DIRECTION('center_axis',(0.,1.,0.));
#2224=DIRECTION('ref_axis',(1.,0.,0.));
#2225=DIRECTION('center_axis',(0.,1.,0.));
#2226=DIRECTION('ref_axis',(1.,0.,0.));
#2227=DIRECTION('axis',(0.,0.,1.));
#2228=DIRECTION('refdir',(1.,0.,0.));
#2229=DIRECTION('center_axis',(0.,1.,0.));
#2230=DIRECTION('ref_axis',(1.,0.,0.));
#2231=DIRECTION('',(0.866025403784439,-0.5,1.06057523872491E-16));
#2232=DIRECTION('center_axis',(0.,-1.,0.));
#2233=DIRECTION('ref_axis',(1.,0.,0.));
#2234=DIRECTION('center_axis',(0.,-1.,0.));
#2235=DIRECTION('ref_axis',(1.,0.,0.));
#2236=DIRECTION('center_axis',(0.,1.,0.));
#2237=DIRECTION('ref_axis',(1.,0.,0.));
#2238=DIRECTION('',(-0.866025403784439,-0.5,-1.06057523872491E-16));
#2239=DIRECTION('center_axis',(1.4792020664489E-16,0.,-1.));
#2240=DIRECTION('ref_axis',(-1.,0.,-1.4792020664489E-16));
#2241=DIRECTION('',(0.,1.,0.));
#2242=DIRECTION('',(0.,1.,0.));
#2243=DIRECTION('center_axis',(-0.866025403784439,0.,-0.5));
#2244=DIRECTION('ref_axis',(-0.5,0.,0.866025403784439));
#2245=DIRECTION('',(0.,1.,0.));
#2246=DIRECTION('center_axis',(-0.866025403784439,0.,0.5));
#2247=DIRECTION('ref_axis',(0.5,0.,0.866025403784439));
#2248=DIRECTION('',(0.,1.,0.));
#2249=DIRECTION('center_axis',(0.,1.,0.));
#2250=DIRECTION('ref_axis',(1.,0.,0.));
#2251=DIRECTION('center_axis',(0.,1.,0.));
#2252=DIRECTION('ref_axis',(1.,0.,0.));
#2253=DIRECTION('',(0.,-1.,0.));
#2254=DIRECTION('center_axis',(0.,1.,0.));
#2255=DIRECTION('ref_axis',(1.,0.,0.));
#2256=DIRECTION('center_axis',(-2.95840413289779E-16,0.,1.));
#2257=DIRECTION('ref_axis',(1.,0.,2.95840413289779E-16));
#2258=DIRECTION('',(0.,1.,0.));
#2259=DIRECTION('center_axis',(0.866025403784439,0.,-0.5));
#2260=DIRECTION('ref_axis',(-0.5,0.,-0.866025403784439));
#2261=DIRECTION('',(0.,1.,0.));
#2262=DIRECTION('center_axis',(0.866025403784439,0.,0.5));
#2263=DIRECTION('ref_axis',(0.5,0.,-0.866025403784439));
#2264=DIRECTION('center_axis',(0.,1.,0.));
#2265=DIRECTION('ref_axis',(1.,0.,0.));
#2266=DIRECTION('center_axis',(0.,1.,0.));
#2267=DIRECTION('ref_axis',(1.,0.,0.));
#2268=DIRECTION('',(0.,0.,1.));
#2269=DIRECTION('',(1.,0.,0.));
#2270=DIRECTION('',(0.,0.,1.));
#2271=DIRECTION('',(1.,0.,0.));
#2272=DIRECTION('',(0.,0.,1.));
#2273=DIRECTION('',(1.,0.,0.));
#2274=DIRECTION('',(0.,0.,1.));
#2275=DIRECTION('',(1.,0.,0.));
#2276=DIRECTION('',(0.,0.,1.));
#2277=DIRECTION('',(1.,0.,0.));
#2278=DIRECTION('',(0.,-1.,2.22044604925031E-16));
#2279=DIRECTION('',(1.,0.,0.));
#2280=DIRECTION('',(0.,-1.,2.22044604925031E-16));
#2281=DIRECTION('',(1.,0.,0.));
#2282=DIRECTION('',(0.,-1.,2.22044604925031E-16));
#2283=DIRECTION('',(1.,0.,0.));
#2284=DIRECTION('',(0.,-1.,2.22044604925031E-16));
#2285=DIRECTION('',(1.,0.,0.));
#2286=CARTESIAN_POINT('',(0.,0.,0.));
#2287=CARTESIAN_POINT('',(0.,0.,0.));
#2288=CARTESIAN_POINT('Origin',(-7.6,-0.5,1.5));
#2289=CARTESIAN_POINT('',(7.5,-0.5,0.9));
#2290=CARTESIAN_POINT('',(7.5,-0.5,1.4));
#2291=CARTESIAN_POINT('',(7.5,-0.5,0.75));
#2292=CARTESIAN_POINT('',(-7.5,-0.5,0.9));
#2293=CARTESIAN_POINT('',(-7.6,-0.5,0.9));
#2294=CARTESIAN_POINT('',(-7.5,-0.5,1.4));
#2295=CARTESIAN_POINT('',(-7.5,-0.5,0.75));
#2296=CARTESIAN_POINT('',(-3.8,-0.5,1.4));
#2297=CARTESIAN_POINT('Origin',(-7.6,-0.5,0.9));
#2298=CARTESIAN_POINT('',(7.5,-0.9,0.9));
#2299=CARTESIAN_POINT('',(7.5,-4.,0.9));
#2300=CARTESIAN_POINT('',(-7.5,-0.9,0.9));
#2301=CARTESIAN_POINT('',(-7.6,-0.9,0.9));
#2302=CARTESIAN_POINT('',(-7.5,3.5,0.9));
#2303=CARTESIAN_POINT('Origin',(-7.6,0.5,0.9));
#2304=CARTESIAN_POINT('',(7.5,0.5,1.4));
#2305=CARTESIAN_POINT('',(7.5,0.5,0.9));
#2306=CARTESIAN_POINT('',(7.5,0.5,0.45));
#2307=CARTESIAN_POINT('',(-7.5,0.5,1.4));
#2308=CARTESIAN_POINT('',(-3.8,0.5,1.4));
#2309=CARTESIAN_POINT('',(-7.5,0.5,0.9));
#2310=CARTESIAN_POINT('',(-7.5,0.5,0.45));
#2311=CARTESIAN_POINT('',(-7.6,0.5,0.9));
#2312=CARTESIAN_POINT('Origin',(-7.6,0.9,0.9));
#2313=CARTESIAN_POINT('',(7.5,0.9,0.9));
#2314=CARTESIAN_POINT('',(7.5,-3.3,0.9));
#2315=CARTESIAN_POINT('',(-7.5,0.9,0.9));
#2316=CARTESIAN_POINT('',(-7.5,4.2,0.9));
#2317=CARTESIAN_POINT('',(-7.6,0.9,0.9));
#2318=CARTESIAN_POINT('Origin',(-7.6,0.9,0.3));
#2319=CARTESIAN_POINT('',(7.5,0.9,0.3));
#2320=CARTESIAN_POINT('',(7.5,0.9,0.15));
#2321=CARTESIAN_POINT('',(-7.5,0.9,0.3));
#2322=CARTESIAN_POINT('',(-7.5,0.9,0.15));
#2323=CARTESIAN_POINT('',(-7.6,0.9,0.3));
#2324=CARTESIAN_POINT('Origin',(-7.6,-0.9,0.3));
#2325=CARTESIAN_POINT('',(7.5,-0.9,0.3));
#2326=CARTESIAN_POINT('',(7.5,-4.2,0.3));
#2327=CARTESIAN_POINT('',(-7.5,-0.9,0.3));
#2328=CARTESIAN_POINT('',(-7.5,3.3,0.3));
#2329=CARTESIAN_POINT('',(-7.6,-0.9,0.3));
#2330=CARTESIAN_POINT('Origin',(-7.6,-0.9,0.9));
#2331=CARTESIAN_POINT('',(7.5,-0.9,0.45));
#2332=CARTESIAN_POINT('',(-7.5,-0.9,0.45));
#2333=CARTESIAN_POINT('Origin',(-7.5,7.5,0.));
#2334=CARTESIAN_POINT('',(-7.5,7.5,1.4));
#2335=CARTESIAN_POINT('',(-7.5,7.5,1.4));
#2336=CARTESIAN_POINT('',(-7.5,7.5,0.));
#2337=CARTESIAN_POINT('',(-7.5,7.5,0.));
#2338=CARTESIAN_POINT('',(-7.5,-7.5,0.));
#2339=CARTESIAN_POINT('',(-7.5,7.5,0.));
#2340=CARTESIAN_POINT('',(-7.5,-7.5,1.4));
#2341=CARTESIAN_POINT('',(-7.5,-7.5,0.));
#2342=CARTESIAN_POINT('',(-7.5,7.5,1.4));
#2343=CARTESIAN_POINT('Origin',(0.,0.,1.4));
#2344=CARTESIAN_POINT('',(7.5,7.5,1.4));
#2345=CARTESIAN_POINT('',(7.5,-7.5,1.4));
#2346=CARTESIAN_POINT('',(7.5,7.5,1.4));
#2347=CARTESIAN_POINT('',(4.66,2.5,1.4));
#2348=CARTESIAN_POINT('Origin',(5.,2.5,1.4));
#2349=CARTESIAN_POINT('',(2.16,2.5,1.4));
#2350=CARTESIAN_POINT('Origin',(2.5,2.5,1.4));
#2351=CARTESIAN_POINT('',(-0.34,2.5,1.4));
#2352=CARTESIAN_POINT('Origin',(0.,2.5,1.4));
#2353=CARTESIAN_POINT('',(-2.84,5.,1.4));
#2354=CARTESIAN_POINT('Origin',(-2.5,5.,1.4));
#2355=CARTESIAN_POINT('',(-5.34,5.,1.4));
#2356=CARTESIAN_POINT('Origin',(-5.,5.,1.4));
#2357=CARTESIAN_POINT('',(-5.34,2.5,1.4));
#2358=CARTESIAN_POINT('Origin',(-5.,2.5,1.4));
#2359=CARTESIAN_POINT('',(-2.84,2.5,1.4));
#2360=CARTESIAN_POINT('Origin',(-2.5,2.5,1.4));
#2361=CARTESIAN_POINT('',(-0.34,5.,1.4));
#2362=CARTESIAN_POINT('Origin',(0.,5.,1.4));
#2363=CARTESIAN_POINT('',(2.16,5.,1.4));
#2364=CARTESIAN_POINT('Origin',(2.5,5.,1.4));
#2365=CARTESIAN_POINT('',(4.66,5.,1.4));
#2366=CARTESIAN_POINT('Origin',(5.,5.,1.4));
#2367=CARTESIAN_POINT('Origin',(0.,0.,1.4));
#2368=CARTESIAN_POINT('',(7.5,-7.5,1.4));
#2369=CARTESIAN_POINT('',(-7.5,-7.5,1.4));
#2370=CARTESIAN_POINT('',(7.5,-7.5,1.4));
#2371=CARTESIAN_POINT('',(4.66,-5.,1.4));
#2372=CARTESIAN_POINT('Origin',(5.,-5.,1.4));
#2373=CARTESIAN_POINT('',(2.16,-5.,1.4));
#2374=CARTESIAN_POINT('Origin',(2.5,-5.,1.4));
#2375=CARTESIAN_POINT('',(-0.34,-2.5,1.4));
#2376=CARTESIAN_POINT('Origin',(0.,-2.5,1.4));
#2377=CARTESIAN_POINT('',(-2.84,-2.5,1.4));
#2378=CARTESIAN_POINT('Origin',(-2.5,-2.5,1.4));
#2379=CARTESIAN_POINT('',(-5.34,-2.5,1.4));
#2380=CARTESIAN_POINT('Origin',(-5.,-2.5,1.4));
#2381=CARTESIAN_POINT('',(-2.84,-5.,1.4));
#2382=CARTESIAN_POINT('Origin',(-2.5,-5.,1.4));
#2383=CARTESIAN_POINT('',(-0.34,-5.,1.4));
#2384=CARTESIAN_POINT('Origin',(0.,-5.,1.4));
#2385=CARTESIAN_POINT('',(-5.34,-5.,1.4));
#2386=CARTESIAN_POINT('Origin',(-5.,-5.,1.4));
#2387=CARTESIAN_POINT('',(2.16,-2.5,1.4));
#2388=CARTESIAN_POINT('Origin',(2.5,-2.5,1.4));
#2389=CARTESIAN_POINT('',(4.66,-2.5,1.4));
#2390=CARTESIAN_POINT('Origin',(5.,-2.5,1.4));
#2391=CARTESIAN_POINT('Origin',(5.,2.5,-0.1));
#2392=CARTESIAN_POINT('',(4.66,2.5,0.));
#2393=CARTESIAN_POINT('Origin',(5.,2.5,0.));
#2394=CARTESIAN_POINT('',(4.66,2.5,-0.1));
#2395=CARTESIAN_POINT('Origin',(5.,-5.,-0.1));
#2396=CARTESIAN_POINT('',(4.66,-5.,0.));
#2397=CARTESIAN_POINT('Origin',(5.,-5.,0.));
#2398=CARTESIAN_POINT('',(4.66,-5.,-0.1));
#2399=CARTESIAN_POINT('Origin',(2.5,2.5,-0.1));
#2400=CARTESIAN_POINT('',(2.16,2.5,0.));
#2401=CARTESIAN_POINT('Origin',(2.5,2.5,0.));
#2402=CARTESIAN_POINT('',(2.16,2.5,-0.1));
#2403=CARTESIAN_POINT('Origin',(2.5,-5.,-0.1));
#2404=CARTESIAN_POINT('',(2.16,-5.,0.));
#2405=CARTESIAN_POINT('Origin',(2.5,-5.,0.));
#2406=CARTESIAN_POINT('',(2.16,-5.,-0.1));
#2407=CARTESIAN_POINT('Origin',(0.,2.5,-0.1));
#2408=CARTESIAN_POINT('',(-0.34,2.5,0.));
#2409=CARTESIAN_POINT('Origin',(0.,2.5,0.));
#2410=CARTESIAN_POINT('',(-0.34,2.5,-0.1));
#2411=CARTESIAN_POINT('Origin',(0.,-2.5,-0.1));
#2412=CARTESIAN_POINT('',(-0.34,-2.5,0.));
#2413=CARTESIAN_POINT('Origin',(0.,-2.5,0.));
#2414=CARTESIAN_POINT('',(-0.34,-2.5,-0.1));
#2415=CARTESIAN_POINT('Origin',(-2.5,5.,-0.1));
#2416=CARTESIAN_POINT('',(-2.84,5.,0.));
#2417=CARTESIAN_POINT('Origin',(-2.5,5.,0.));
#2418=CARTESIAN_POINT('',(-2.84,5.,-0.1));
#2419=CARTESIAN_POINT('Origin',(-2.5,-2.5,-0.1));
#2420=CARTESIAN_POINT('',(-2.84,-2.5,0.));
#2421=CARTESIAN_POINT('Origin',(-2.5,-2.5,0.));
#2422=CARTESIAN_POINT('',(-2.84,-2.5,-0.1));
#2423=CARTESIAN_POINT('Origin',(-5.,5.,-0.1));
#2424=CARTESIAN_POINT('',(-5.34,5.,0.));
#2425=CARTESIAN_POINT('Origin',(-5.,5.,0.));
#2426=CARTESIAN_POINT('',(-5.34,5.,-0.1));
#2427=CARTESIAN_POINT('Origin',(-5.,-2.5,-0.1));
#2428=CARTESIAN_POINT('',(-5.34,-2.5,0.));
#2429=CARTESIAN_POINT('Origin',(-5.,-2.5,0.));
#2430=CARTESIAN_POINT('',(-5.34,-2.5,-0.1));
#2431=CARTESIAN_POINT('Origin',(-5.,2.5,-0.1));
#2432=CARTESIAN_POINT('',(-5.34,2.5,0.));
#2433=CARTESIAN_POINT('Origin',(-5.,2.5,0.));
#2434=CARTESIAN_POINT('',(-5.34,2.5,-0.1));
#2435=CARTESIAN_POINT('Origin',(-2.5,-5.,-0.1));
#2436=CARTESIAN_POINT('',(-2.84,-5.,0.));
#2437=CARTESIAN_POINT('Origin',(-2.5,-5.,0.));
#2438=CARTESIAN_POINT('',(-2.84,-5.,-0.1));
#2439=CARTESIAN_POINT('Origin',(-2.5,2.5,-0.1));
#2440=CARTESIAN_POINT('',(-2.84,2.5,0.));
#2441=CARTESIAN_POINT('Origin',(-2.5,2.5,0.));
#2442=CARTESIAN_POINT('',(-2.84,2.5,-0.1));
#2443=CARTESIAN_POINT('Origin',(0.,-5.,-0.1));
#2444=CARTESIAN_POINT('',(-0.34,-5.,0.));
#2445=CARTESIAN_POINT('Origin',(0.,-5.,0.));
#2446=CARTESIAN_POINT('',(-0.34,-5.,-0.1));
#2447=CARTESIAN_POINT('Origin',(-5.,-5.,-0.1));
#2448=CARTESIAN_POINT('',(-5.34,-5.,0.));
#2449=CARTESIAN_POINT('Origin',(-5.,-5.,0.));
#2450=CARTESIAN_POINT('',(-5.34,-5.,-0.1));
#2451=CARTESIAN_POINT('Origin',(0.,5.,-0.1));
#2452=CARTESIAN_POINT('',(-0.34,5.,0.));
#2453=CARTESIAN_POINT('Origin',(0.,5.,0.));
#2454=CARTESIAN_POINT('',(-0.34,5.,-0.1));
#2455=CARTESIAN_POINT('Origin',(2.5,-2.5,-0.1));
#2456=CARTESIAN_POINT('',(2.16,-2.5,0.));
#2457=CARTESIAN_POINT('Origin',(2.5,-2.5,0.));
#2458=CARTESIAN_POINT('',(2.16,-2.5,-0.1));
#2459=CARTESIAN_POINT('Origin',(2.5,5.,-0.1));
#2460=CARTESIAN_POINT('',(2.16,5.,0.));
#2461=CARTESIAN_POINT('Origin',(2.5,5.,0.));
#2462=CARTESIAN_POINT('',(2.16,5.,-0.1));
#2463=CARTESIAN_POINT('Origin',(5.,-2.5,-0.1));
#2464=CARTESIAN_POINT('',(4.66,-2.5,0.));
#2465=CARTESIAN_POINT('Origin',(5.,-2.5,0.));
#2466=CARTESIAN_POINT('',(4.66,-2.5,-0.1));
#2467=CARTESIAN_POINT('Origin',(5.,5.,-0.1));
#2468=CARTESIAN_POINT('',(4.66,5.,0.));
#2469=CARTESIAN_POINT('Origin',(5.,5.,0.));
#2470=CARTESIAN_POINT('',(4.66,5.,-0.1));
#2471=CARTESIAN_POINT('Origin',(7.5,7.5,0.));
#2472=CARTESIAN_POINT('',(7.5,7.5,0.));
#2473=CARTESIAN_POINT('',(7.5,7.5,0.));
#2474=CARTESIAN_POINT('',(7.5,7.5,0.));
#2475=CARTESIAN_POINT('Origin',(7.5,-7.5,0.));
#2476=CARTESIAN_POINT('',(7.5,-7.5,0.));
#2477=CARTESIAN_POINT('',(7.5,-7.5,0.));
#2478=CARTESIAN_POINT('',(7.5,-7.5,0.));
#2479=CARTESIAN_POINT('Origin',(-7.5,-7.5,0.));
#2480=CARTESIAN_POINT('',(-7.5,-7.5,0.));
#2481=CARTESIAN_POINT('Origin',(0.,0.,0.));
#2482=CARTESIAN_POINT('',(0.,0.,0.));
#2483=CARTESIAN_POINT('Origin',(0.,0.,0.2));
#2484=CARTESIAN_POINT('',(-0.34,-4.163799117101E-17,0.3));
#2485=CARTESIAN_POINT('Origin',(0.,0.,0.3));
#2486=CARTESIAN_POINT('',(-0.34,4.163799117101E-17,1.4));
#2487=CARTESIAN_POINT('',(-0.34,-4.163799117101E-17,0.2));
#2488=CARTESIAN_POINT('Origin',(0.,0.,1.4));
#2489=CARTESIAN_POINT('Origin',(1.,0.45,0.9));
#2490=CARTESIAN_POINT('',(-1.,0.45,0.9));
#2491=CARTESIAN_POINT('',(1.,0.45,0.9));
#2492=CARTESIAN_POINT('',(0.5,0.45,0.9));
#2493=CARTESIAN_POINT('',(-1.,0.45,1.4));
#2494=CARTESIAN_POINT('',(-1.,0.45,0.9));
#2495=CARTESIAN_POINT('',(1.,0.45,1.4));
#2496=CARTESIAN_POINT('',(1.,0.45,1.4));
#2497=CARTESIAN_POINT('',(1.,0.45,0.9));
#2498=CARTESIAN_POINT('Origin',(-1.,-0.45,0.9));
#2499=CARTESIAN_POINT('',(1.,-0.45,0.9));
#2500=CARTESIAN_POINT('',(-1.,-0.45,0.9));
#2501=CARTESIAN_POINT('',(-0.5,-0.45,0.9));
#2502=CARTESIAN_POINT('',(1.,-0.45,1.4));
#2503=CARTESIAN_POINT('',(1.,-0.45,0.9));
#2504=CARTESIAN_POINT('',(-1.,-0.45,1.4));
#2505=CARTESIAN_POINT('',(-1.,-0.45,1.4));
#2506=CARTESIAN_POINT('',(-1.,-0.45,0.9));
#2507=CARTESIAN_POINT('Origin',(0.,0.,1.4));
#2508=CARTESIAN_POINT('',(-1.,0.45,1.4));
#2509=CARTESIAN_POINT('',(1.,-0.45,1.4));
#2510=CARTESIAN_POINT('Origin',(0.,0.,0.9));
#2511=CARTESIAN_POINT('',(1.,0.8,0.9));
#2512=CARTESIAN_POINT('',(1.,-0.8,0.9));
#2513=CARTESIAN_POINT('',(-1.,0.8,0.9));
#2514=CARTESIAN_POINT('',(1.,0.8,0.9));
#2515=CARTESIAN_POINT('',(-1.,0.8,0.9));
#2516=CARTESIAN_POINT('Origin',(0.,0.,0.9));
#2517=CARTESIAN_POINT('',(-1.,-0.8,0.9));
#2518=CARTESIAN_POINT('',(-1.,0.8,0.9));
#2519=CARTESIAN_POINT('',(1.,-0.8,0.9));
#2520=CARTESIAN_POINT('',(-1.,-0.8,0.9));
#2521=CARTESIAN_POINT('',(1.,-0.8,0.9));
#2522=CARTESIAN_POINT('Origin',(1.,0.8,0.3));
#2523=CARTESIAN_POINT('',(1.,0.8,0.3));
#2524=CARTESIAN_POINT('',(-1.,0.8,0.3));
#2525=CARTESIAN_POINT('',(1.,0.8,0.3));
#2526=CARTESIAN_POINT('',(-1.,0.8,0.3));
#2527=CARTESIAN_POINT('',(1.,0.8,0.3));
#2528=CARTESIAN_POINT('Origin',(1.,-0.8,0.3));
#2529=CARTESIAN_POINT('',(1.,-0.8,0.3));
#2530=CARTESIAN_POINT('',(1.,-0.8,0.3));
#2531=CARTESIAN_POINT('',(1.,-0.8,0.3));
#2532=CARTESIAN_POINT('Origin',(-1.,-0.8,0.3));
#2533=CARTESIAN_POINT('',(-1.,-0.8,0.3));
#2534=CARTESIAN_POINT('',(-1.,-0.8,0.3));
#2535=CARTESIAN_POINT('',(-1.,-0.8,0.3));
#2536=CARTESIAN_POINT('Origin',(-1.,0.8,0.3));
#2537=CARTESIAN_POINT('',(-1.,0.8,0.3));
#2538=CARTESIAN_POINT('Origin',(0.,0.,0.3));
#2539=CARTESIAN_POINT('',(0.,0.,0.));
#2540=CARTESIAN_POINT('Origin',(2.,-1.5,1.4));
#2541=CARTESIAN_POINT('',(2.,-1.5,3.8));
#2542=CARTESIAN_POINT('',(2.,-1.5,1.4));
#2543=CARTESIAN_POINT('',(2.,-1.5,3.8));
#2544=CARTESIAN_POINT('',(2.,1.5,3.8));
#2545=CARTESIAN_POINT('',(2.,-1.5,3.8));
#2546=CARTESIAN_POINT('',(2.,1.5,1.4));
#2547=CARTESIAN_POINT('',(2.,1.5,3.8));
#2548=CARTESIAN_POINT('',(2.,-1.5,1.4));
#2549=CARTESIAN_POINT('Origin',(5.5,-1.5,1.4));
#2550=CARTESIAN_POINT('',(5.5,-1.5,1.4));
#2551=CARTESIAN_POINT('',(2.,-1.5,1.4));
#2552=CARTESIAN_POINT('',(5.5,1.5,1.4));
#2553=CARTESIAN_POINT('',(2.,1.5,1.4));
#2554=CARTESIAN_POINT('',(5.5,-1.5,1.4));
#2555=CARTESIAN_POINT('Origin',(5.5,-1.5,5.8));
#2556=CARTESIAN_POINT('',(5.5,-1.5,5.8));
#2557=CARTESIAN_POINT('',(5.5,-1.5,1.4));
#2558=CARTESIAN_POINT('',(5.5,1.5,5.8));
#2559=CARTESIAN_POINT('',(5.5,1.5,1.4));
#2560=CARTESIAN_POINT('',(5.5,-1.5,5.8));
#2561=CARTESIAN_POINT('Origin',(4.,-1.5,5.8));
#2562=CARTESIAN_POINT('',(4.,-1.5,5.8));
#2563=CARTESIAN_POINT('',(5.5,-1.5,5.8));
#2564=CARTESIAN_POINT('',(4.,1.5,5.8));
#2565=CARTESIAN_POINT('',(5.5,1.5,5.8));
#2566=CARTESIAN_POINT('',(4.,-1.5,5.8));
#2567=CARTESIAN_POINT('Origin',(4.,-1.5,4.8));
#2568=CARTESIAN_POINT('',(4.,-1.5,4.8));
#2569=CARTESIAN_POINT('',(4.,-1.5,5.8));
#2570=CARTESIAN_POINT('',(4.,1.5,4.8));
#2571=CARTESIAN_POINT('',(4.,1.5,5.8));
#2572=CARTESIAN_POINT('',(4.,-1.5,4.8));
#2573=CARTESIAN_POINT('Origin',(3.,-1.5,4.8));
#2574=CARTESIAN_POINT('',(3.,-1.5,4.8));
#2575=CARTESIAN_POINT('',(4.,-1.5,4.8));
#2576=CARTESIAN_POINT('',(3.,1.5,4.8));
#2577=CARTESIAN_POINT('',(4.,1.5,4.8));
#2578=CARTESIAN_POINT('',(3.,-1.5,4.8));
#2579=CARTESIAN_POINT('Origin',(3.,-1.5,3.8));
#2580=CARTESIAN_POINT('',(3.,-1.5,3.8));
#2581=CARTESIAN_POINT('',(3.,-1.5,4.8));
#2582=CARTESIAN_POINT('',(3.,1.5,3.8));
#2583=CARTESIAN_POINT('',(3.,1.5,4.8));
#2584=CARTESIAN_POINT('',(3.,-1.5,3.8));
#2585=CARTESIAN_POINT('Origin',(2.,-1.5,3.8));
#2586=CARTESIAN_POINT('',(3.,-1.5,3.8));
#2587=CARTESIAN_POINT('',(3.,1.5,3.8));
#2588=CARTESIAN_POINT('Origin',(3.75,1.5,3.6));
#2589=CARTESIAN_POINT('Origin',(3.75,-1.5,3.6));
#2590=CARTESIAN_POINT('',(0.,0.,0.));
#2591=CARTESIAN_POINT('Origin',(0.4,0.45,5.7));
#2592=CARTESIAN_POINT('',(0.4,0.45,5.8));
#2593=CARTESIAN_POINT('',(-0.4,0.45,5.8));
#2594=CARTESIAN_POINT('',(0.2,0.45,5.8));
#2595=CARTESIAN_POINT('',(0.4,0.45,6.6));
#2596=CARTESIAN_POINT('',(0.4,0.45,5.7));
#2597=CARTESIAN_POINT('',(-0.4,0.45,6.6));
#2598=CARTESIAN_POINT('',(0.2,0.45,6.6));
#2599=CARTESIAN_POINT('',(-0.4,0.45,5.7));
#2600=CARTESIAN_POINT('Origin',(-0.4,-0.45,5.7));
#2601=CARTESIAN_POINT('',(-0.4,-0.45,5.8));
#2602=CARTESIAN_POINT('',(0.4,-0.45,5.8));
#2603=CARTESIAN_POINT('',(-0.2,-0.45,5.8));
#2604=CARTESIAN_POINT('',(-0.4,-0.45,6.6));
#2605=CARTESIAN_POINT('',(-0.4,-0.45,5.7));
#2606=CARTESIAN_POINT('',(0.4,-0.45,6.6));
#2607=CARTESIAN_POINT('',(-0.2,-0.45,6.6));
#2608=CARTESIAN_POINT('',(0.4,-0.45,5.7));
#2609=CARTESIAN_POINT('Origin',(0.,0.,5.8));
#2610=CARTESIAN_POINT('',(-5.,1.2,5.8));
#2611=CARTESIAN_POINT('',(-5.,-1.2,5.8));
#2612=CARTESIAN_POINT('',(-5.,1.2,5.8));
#2613=CARTESIAN_POINT('',(5.,1.2,5.8));
#2614=CARTESIAN_POINT('',(5.,1.2,5.8));
#2615=CARTESIAN_POINT('',(5.,-1.2,5.8));
#2616=CARTESIAN_POINT('',(5.,-1.2,5.8));
#2617=CARTESIAN_POINT('',(-5.,-1.2,5.8));
#2618=CARTESIAN_POINT('Origin',(-0.4,0.,5.8));
#2619=CARTESIAN_POINT('Origin',(0.4,0.,5.8));
#2620=CARTESIAN_POINT('Origin',(-0.4,0.,5.7));
#2621=CARTESIAN_POINT('Origin',(-0.4,0.,6.6));
#2622=CARTESIAN_POINT('Origin',(0.4,0.,5.7));
#2623=CARTESIAN_POINT('Origin',(0.4,0.,6.6));
#2624=CARTESIAN_POINT('Origin',(5.,1.2,5.8));
#2625=CARTESIAN_POINT('',(-5.,1.2,6.6));
#2626=CARTESIAN_POINT('',(-5.,1.2,5.8));
#2627=CARTESIAN_POINT('',(5.,1.2,6.6));
#2628=CARTESIAN_POINT('',(5.,1.2,6.6));
#2629=CARTESIAN_POINT('',(5.,1.2,5.8));
#2630=CARTESIAN_POINT('Origin',(5.,-1.2,5.8));
#2631=CARTESIAN_POINT('',(5.,-1.2,6.6));
#2632=CARTESIAN_POINT('',(5.,-1.2,6.6));
#2633=CARTESIAN_POINT('',(5.,-1.2,5.8));
#2634=CARTESIAN_POINT('Origin',(-5.,-1.2,5.8));
#2635=CARTESIAN_POINT('',(-5.,-1.2,6.6));
#2636=CARTESIAN_POINT('',(-5.,-1.2,6.6));
#2637=CARTESIAN_POINT('',(-5.,-1.2,5.8));
#2638=CARTESIAN_POINT('Origin',(-5.,1.2,5.8));
#2639=CARTESIAN_POINT('',(-5.,1.2,6.6));
#2640=CARTESIAN_POINT('Origin',(0.,0.,6.6));
#2641=CARTESIAN_POINT('',(0.,0.,0.));
#2642=CARTESIAN_POINT('Origin',(10.,-4.,0.));
#2643=CARTESIAN_POINT('',(9.6067,-4.,8.3));
#2644=CARTESIAN_POINT('Origin',(10.,-4.,8.3));
#2645=CARTESIAN_POINT('',(9.6067,-4.,0.));
#2646=CARTESIAN_POINT('',(9.6067,-4.,0.));
#2647=CARTESIAN_POINT('Origin',(10.,-4.,0.));
#2648=CARTESIAN_POINT('Origin',(10.,-4.,8.3));
#2649=CARTESIAN_POINT('Origin',(10.,-4.,0.));
#2650=CARTESIAN_POINT('',(0.,0.,0.));
#2651=CARTESIAN_POINT('Origin',(0.,0.,0.));
#2652=CARTESIAN_POINT('',(-0.42,0.16,5.14351655641888E-17));
#2653=CARTESIAN_POINT('Origin',(0.,0.16,0.));
#2654=CARTESIAN_POINT('',(-0.42,0.,5.14351655641888E-17));
#2655=CARTESIAN_POINT('',(-0.42,0.,5.14351655641888E-17));
#2656=CARTESIAN_POINT('Origin',(0.,0.,0.));
#2657=CARTESIAN_POINT('Origin',(0.,0.,0.));
#2658=CARTESIAN_POINT('',(-0.8,0.16,9.79717439317883E-17));
#2659=CARTESIAN_POINT('Origin',(0.,0.16,0.));
#2660=CARTESIAN_POINT('',(-0.8,0.,9.79717439317883E-17));
#2661=CARTESIAN_POINT('',(-0.8,0.,9.79717439317883E-17));
#2662=CARTESIAN_POINT('Origin',(0.,0.,0.));
#2663=CARTESIAN_POINT('Origin',(0.,0.16,0.));
#2664=CARTESIAN_POINT('Origin',(0.,0.,0.));
#2665=CARTESIAN_POINT('',(0.,0.,0.));
#2666=CARTESIAN_POINT('Origin',(0.,0.067277284513851,0.));
#2667=CARTESIAN_POINT('',(-0.375277674973257,0.0768195421087395,0.65));
#2668=CARTESIAN_POINT('',(0.375277674973257,0.0768195421087395,0.65));
#2669=CARTESIAN_POINT('Ctrl Pts',(-0.375277674973257,0.0768195421087395,
0.65));
#2670=CARTESIAN_POINT('Ctrl Pts',(1.66533453693773E-13,-0.0315137912242439,
0.65));
#2671=CARTESIAN_POINT('Ctrl Pts',(0.375277674973257,0.0768195421087394,
0.65));
#2672=CARTESIAN_POINT('',(-0.750555349946514,0.0768195421087394,-9.19165206894919E-17));
#2673=CARTESIAN_POINT('Ctrl Pts',(-0.750555349946514,0.0768195421087394,
-9.19165206894919E-17));
#2674=CARTESIAN_POINT('Ctrl Pts',(-0.562916512459802,-0.0315137912242434,
0.325000000000144));
#2675=CARTESIAN_POINT('Ctrl Pts',(-0.375277674973257,0.0768195421087395,
0.65));
#2676=CARTESIAN_POINT('',(-0.6175,-2.77555756156289E-17,-7.5621939847349E-17));
#2677=CARTESIAN_POINT('',(-0.734027674973257,0.067277284513851,-8.98924642641573E-17));
#2678=CARTESIAN_POINT('Origin',(0.,0.,0.));
#2679=CARTESIAN_POINT('',(-0.375277674973257,0.0768195421087395,-0.65));
#2680=CARTESIAN_POINT('Ctrl Pts',(-0.375277674973257,0.0768195421087395,
-0.65));
#2681=CARTESIAN_POINT('Ctrl Pts',(-0.562916512459968,-0.0315137912242437,
-0.324999999999856));
#2682=CARTESIAN_POINT('Ctrl Pts',(-0.750555349946514,0.0768195421087395,
-9.19165206894919E-17));
#2683=CARTESIAN_POINT('',(0.375277674973257,0.0768195421087395,-0.65));
#2684=CARTESIAN_POINT('Ctrl Pts',(0.375277674973257,0.0768195421087395,
-0.65));
#2685=CARTESIAN_POINT('Ctrl Pts',(-1.66144875635155E-13,-0.0315137912242437,
-0.65));
#2686=CARTESIAN_POINT('Ctrl Pts',(-0.375277674973257,0.0768195421087395,
-0.65));
#2687=CARTESIAN_POINT('',(0.750555349946514,0.0768195421087394,0.));
#2688=CARTESIAN_POINT('Ctrl Pts',(0.750555349946514,0.0768195421087394,
0.));
#2689=CARTESIAN_POINT('Ctrl Pts',(0.562916512459802,-0.0315137912242436,
-0.325000000000144));
#2690=CARTESIAN_POINT('Ctrl Pts',(0.375277674973257,0.0768195421087395,
-0.65));
#2691=CARTESIAN_POINT('Ctrl Pts',(0.375277674973257,0.0768195421087394,
0.65));
#2692=CARTESIAN_POINT('Ctrl Pts',(0.562916512459968,-0.0315137912242439,
0.324999999999856));
#2693=CARTESIAN_POINT('Ctrl Pts',(0.750555349946514,0.0768195421087394,
0.));
#2694=CARTESIAN_POINT('Origin',(0.,0.612722715486149,0.));
#2695=CARTESIAN_POINT('',(-0.6175,0.68,-7.5621939847349E-17));
#2696=CARTESIAN_POINT('Origin',(0.,0.68,0.));
#2697=CARTESIAN_POINT('',(-0.750555349946514,0.603180457891261,-9.19165206894919E-17));
#2698=CARTESIAN_POINT('',(-0.734027674973257,0.612722715486149,-8.98924642641573E-17));
#2699=CARTESIAN_POINT('',(-0.375277674973257,0.603180457891261,0.65));
#2700=CARTESIAN_POINT('Ctrl Pts',(-0.375277674973257,0.603180457891261,
0.65));
#2701=CARTESIAN_POINT('Ctrl Pts',(-0.562916512459968,0.711513791224243,
0.324999999999856));
#2702=CARTESIAN_POINT('Ctrl Pts',(-0.750555349946514,0.603180457891261,
-9.19165206894919E-17));
#2703=CARTESIAN_POINT('',(0.375277674973257,0.603180457891261,0.65));
#2704=CARTESIAN_POINT('Ctrl Pts',(0.375277674973257,0.603180457891261,0.65));
#2705=CARTESIAN_POINT('Ctrl Pts',(-1.66755498298699E-13,0.711513791224244,
0.65));
#2706=CARTESIAN_POINT('Ctrl Pts',(-0.375277674973257,0.603180457891261,
0.65));
#2707=CARTESIAN_POINT('',(0.750555349946514,0.603180457891261,0.));
#2708=CARTESIAN_POINT('Ctrl Pts',(0.750555349946514,0.603180457891261,0.));
#2709=CARTESIAN_POINT('Ctrl Pts',(0.562916512459802,0.711513791224244,0.325000000000144));
#2710=CARTESIAN_POINT('Ctrl Pts',(0.375277674973257,0.603180457891261,0.65));
#2711=CARTESIAN_POINT('',(0.375277674973257,0.603180457891261,-0.65));
#2712=CARTESIAN_POINT('Ctrl Pts',(0.375277674973257,0.603180457891261,-0.65));
#2713=CARTESIAN_POINT('Ctrl Pts',(0.562916512459969,0.711513791224244,-0.324999999999856));
#2714=CARTESIAN_POINT('Ctrl Pts',(0.750555349946514,0.603180457891261,0.));
#2715=CARTESIAN_POINT('',(-0.375277674973257,0.603180457891261,-0.65));
#2716=CARTESIAN_POINT('Ctrl Pts',(-0.375277674973257,0.603180457891261,
-0.65));
#2717=CARTESIAN_POINT('Ctrl Pts',(1.66422431391311E-13,0.711513791224244,
-0.65));
#2718=CARTESIAN_POINT('Ctrl Pts',(0.375277674973257,0.603180457891261,-0.65));
#2719=CARTESIAN_POINT('Ctrl Pts',(-0.750555349946514,0.603180457891261,
-9.19165206894919E-17));
#2720=CARTESIAN_POINT('Ctrl Pts',(-0.562916512459802,0.711513791224244,
-0.325000000000144));
#2721=CARTESIAN_POINT('Ctrl Pts',(-0.375277674973257,0.603180457891261,
-0.65));
#2722=CARTESIAN_POINT('Origin',(0.375277674973257,0.,-0.65));
#2723=CARTESIAN_POINT('',(-0.375277674973257,0.,-0.65));
#2724=CARTESIAN_POINT('',(0.375277674973257,0.,-0.65));
#2725=CARTESIAN_POINT('Origin',(-0.375277674973257,0.,-0.65));
#2726=CARTESIAN_POINT('',(-0.750555349946514,0.,-9.19165206894919E-17));
#2727=CARTESIAN_POINT('Origin',(-0.750555349946514,0.,-9.19165206894919E-17));
#2728=CARTESIAN_POINT('',(-0.375277674973257,0.,0.65));
#2729=CARTESIAN_POINT('Origin',(0.,0.,0.));
#2730=CARTESIAN_POINT('',(-0.338975,0.68,4.15124648740974E-17));
#2731=CARTESIAN_POINT('Origin',(0.,0.68,0.));
#2732=CARTESIAN_POINT('',(-0.338975,0.,4.15124648740974E-17));
#2733=CARTESIAN_POINT('',(-0.338975,0.,4.15124648740974E-17));
#2734=CARTESIAN_POINT('Origin',(0.,0.,0.));
#2735=CARTESIAN_POINT('Origin',(-0.375277674973257,0.,0.65));
#2736=CARTESIAN_POINT('',(0.375277674973257,0.,0.65));
#2737=CARTESIAN_POINT('Origin',(0.750555349946514,0.,0.));
#2738=CARTESIAN_POINT('',(0.750555349946514,0.,0.));
#2739=CARTESIAN_POINT('Origin',(0.375277674973257,0.,0.65));
#2740=CARTESIAN_POINT('Origin',(0.,0.68,-1.11022302462516E-16));
#2741=CARTESIAN_POINT('Origin',(0.,0.,-1.11022302462516E-16));
#2742=CARTESIAN_POINT('',(0.,0.,0.));
#2743=CARTESIAN_POINT('',(0.,0.,0.));
#2744=CARTESIAN_POINT('',(0.,0.,0.));
#2745=CARTESIAN_POINT('',(0.,0.,0.));
#2746=CARTESIAN_POINT('',(-10.,4.,0.3));
#2747=CARTESIAN_POINT('',(0.,0.,1.4));
#2748=CARTESIAN_POINT('',(0.,0.,1.56));
#2749=CARTESIAN_POINT('',(0.,0.,6.6));
#2750=CARTESIAN_POINT('',(0.,0.,6.76));
#2751=UNCERTAINTY_MEASURE_WITH_UNIT(LENGTH_MEASURE(0.001),#2769,
'DISTANCE_ACCURACY_VALUE',
'Maximum model space distance between geometric entities at asserted c
onnectivities');
#2752=UNCERTAINTY_MEASURE_WITH_UNIT(LENGTH_MEASURE(0.001),#2769,
'DISTANCE_ACCURACY_VALUE',
'Maximum model space distance between geometric entities at asserted c
onnectivities');
#2753=UNCERTAINTY_MEASURE_WITH_UNIT(LENGTH_MEASURE(0.001),#2769,
'DISTANCE_ACCURACY_VALUE',
'Maximum model space distance between geometric entities at asserted c
onnectivities');
#2754=UNCERTAINTY_MEASURE_WITH_UNIT(LENGTH_MEASURE(0.001),#2769,
'DISTANCE_ACCURACY_VALUE',
'Maximum model space distance between geometric entities at asserted c
onnectivities');
#2755=UNCERTAINTY_MEASURE_WITH_UNIT(LENGTH_MEASURE(0.001),#2769,
'DISTANCE_ACCURACY_VALUE',
'Maximum model space distance between geometric entities at asserted c
onnectivities');
#2756=UNCERTAINTY_MEASURE_WITH_UNIT(LENGTH_MEASURE(0.001),#2769,
'DISTANCE_ACCURACY_VALUE',
'Maximum model space distance between geometric entities at asserted c
onnectivities');
#2757=UNCERTAINTY_MEASURE_WITH_UNIT(LENGTH_MEASURE(0.001),#2769,
'DISTANCE_ACCURACY_VALUE',
'Maximum model space distance between geometric entities at asserted c
onnectivities');
#2758=UNCERTAINTY_MEASURE_WITH_UNIT(LENGTH_MEASURE(0.001),#2769,
'DISTANCE_ACCURACY_VALUE',
'Maximum model space distance between geometric entities at asserted c
onnectivities');
#2759=UNCERTAINTY_MEASURE_WITH_UNIT(LENGTH_MEASURE(0.001),#2769,
'DISTANCE_ACCURACY_VALUE',
'Maximum model space distance between geometric entities at asserted c
onnectivities');
#2760=(
GEOMETRIC_REPRESENTATION_CONTEXT(3)
GLOBAL_UNCERTAINTY_ASSIGNED_CONTEXT((#2751))
GLOBAL_UNIT_ASSIGNED_CONTEXT((#2769,#2771,#2772))
REPRESENTATION_CONTEXT('','3D')
);
#2761=(
GEOMETRIC_REPRESENTATION_CONTEXT(3)
GLOBAL_UNCERTAINTY_ASSIGNED_CONTEXT((#2752))
GLOBAL_UNIT_ASSIGNED_CONTEXT((#2769,#2771,#2772))
REPRESENTATION_CONTEXT('','3D')
);
#2762=(
GEOMETRIC_REPRESENTATION_CONTEXT(3)
GLOBAL_UNCERTAINTY_ASSIGNED_CONTEXT((#2753))
GLOBAL_UNIT_ASSIGNED_CONTEXT((#2769,#2771,#2772))
REPRESENTATION_CONTEXT('','3D')
);
#2763=(
GEOMETRIC_REPRESENTATION_CONTEXT(3)
GLOBAL_UNCERTAINTY_ASSIGNED_CONTEXT((#2754))
GLOBAL_UNIT_ASSIGNED_CONTEXT((#2769,#2771,#2772))
REPRESENTATION_CONTEXT('','3D')
);
#2764=(
GEOMETRIC_REPRESENTATION_CONTEXT(3)
GLOBAL_UNCERTAINTY_ASSIGNED_CONTEXT((#2755))
GLOBAL_UNIT_ASSIGNED_CONTEXT((#2769,#2771,#2772))
REPRESENTATION_CONTEXT('','3D')
);
#2765=(
GEOMETRIC_REPRESENTATION_CONTEXT(3)
GLOBAL_UNCERTAINTY_ASSIGNED_CONTEXT((#2756))
GLOBAL_UNIT_ASSIGNED_CONTEXT((#2769,#2771,#2772))
REPRESENTATION_CONTEXT('','3D')
);
#2766=(
GEOMETRIC_REPRESENTATION_CONTEXT(3)
GLOBAL_UNCERTAINTY_ASSIGNED_CONTEXT((#2757))
GLOBAL_UNIT_ASSIGNED_CONTEXT((#2769,#2771,#2772))
REPRESENTATION_CONTEXT('','3D')
);
#2767=(
GEOMETRIC_REPRESENTATION_CONTEXT(3)
GLOBAL_UNCERTAINTY_ASSIGNED_CONTEXT((#2758))
GLOBAL_UNIT_ASSIGNED_CONTEXT((#2769,#2771,#2772))
REPRESENTATION_CONTEXT('','3D')
);
#2768=(
GEOMETRIC_REPRESENTATION_CONTEXT(3)
GLOBAL_UNCERTAINTY_ASSIGNED_CONTEXT((#2759))
GLOBAL_UNIT_ASSIGNED_CONTEXT((#2769,#2771,#2772))
REPRESENTATION_CONTEXT('','3D')
);
#2769=(
LENGTH_UNIT()
NAMED_UNIT(*)
SI_UNIT(.CENTI.,.METRE.)
);
#2770=(
LENGTH_UNIT()
NAMED_UNIT(*)
SI_UNIT($,.METRE.)
);
#2771=(
NAMED_UNIT(*)
PLANE_ANGLE_UNIT()
SI_UNIT($,.RADIAN.)
);
#2772=(
NAMED_UNIT(*)
SI_UNIT($,.STERADIAN.)
SOLID_ANGLE_UNIT()
);
#2773=SHAPE_DEFINITION_REPRESENTATION(#2781,#2798);
#2774=SHAPE_DEFINITION_REPRESENTATION(#2782,#2799);
#2775=SHAPE_DEFINITION_REPRESENTATION(#2783,#2800);
#2776=SHAPE_DEFINITION_REPRESENTATION(#2784,#2801);
#2777=SHAPE_DEFINITION_REPRESENTATION(#2785,#2802);
#2778=SHAPE_DEFINITION_REPRESENTATION(#2786,#2803);
#2779=SHAPE_DEFINITION_REPRESENTATION(#2787,#2804);
#2780=SHAPE_DEFINITION_REPRESENTATION(#2788,#2805);
#2781=PRODUCT_DEFINITION_SHAPE('',$,#2807);
#2782=PRODUCT_DEFINITION_SHAPE('',$,#2808);
#2783=PRODUCT_DEFINITION_SHAPE('',$,#2809);
#2784=PRODUCT_DEFINITION_SHAPE('',$,#2810);
#2785=PRODUCT_DEFINITION_SHAPE('',$,#2811);
#2786=PRODUCT_DEFINITION_SHAPE('',$,#2812);
#2787=PRODUCT_DEFINITION_SHAPE('',$,#2813);
#2788=PRODUCT_DEFINITION_SHAPE('',$,#2814);
#2789=PRODUCT_DEFINITION_SHAPE($,$,#38);
#2790=PRODUCT_DEFINITION_SHAPE($,$,#39);
#2791=PRODUCT_DEFINITION_SHAPE($,$,#40);
#2792=PRODUCT_DEFINITION_SHAPE($,$,#41);
#2793=PRODUCT_DEFINITION_SHAPE($,$,#42);
#2794=PRODUCT_DEFINITION_SHAPE($,$,#43);
#2795=PRODUCT_DEFINITION_SHAPE($,$,#44);
#2796=PRODUCT_DEFINITION_SHAPE($,$,#45);
#2797=PRODUCT_DEFINITION_SHAPE($,$,#46);
#2798=SHAPE_REPRESENTATION('',(#1681,#1828,#1829,#1830,#1831,#1832,#1833,
#1834,#1835,#1836),#2760);
#2799=SHAPE_REPRESENTATION('',(#1682),#2761);
#2800=SHAPE_REPRESENTATION('',(#1757),#2762);
#2801=SHAPE_REPRESENTATION('',(#1771),#2763);
#2802=SHAPE_REPRESENTATION('',(#1782),#2764);
#2803=SHAPE_REPRESENTATION('',(#1797),#2765);
#2804=SHAPE_REPRESENTATION('',(#1803),#2766);
#2805=SHAPE_REPRESENTATION('',(#1812),#2767);
#2806=PRODUCT_DEFINITION_CONTEXT('part definition',#2832,'design');
#2807=PRODUCT_DEFINITION('PAT-097',
'PAT-097',#2815,#2806);
#2808=PRODUCT_DEFINITION('Slotted grid plate','Slotted grid plate',
#2816,#2806);
#2809=PRODUCT_DEFINITION('M8 captive slot nut',
'M8 captive slot nut',#2817,#2806);
#2810=PRODUCT_DEFINITION('Stepped heel block',
'Stepped heel block',#2818,#2806);
#2811=PRODUCT_DEFINITION('Slotted clamp strap',
'Slotted clamp strap',#2819,#2806);
#2812=PRODUCT_DEFINITION('M8 clamp stud','M8 clamp stud',#2820,
#2806);
#2813=PRODUCT_DEFINITION('Flat Washer - M8','Flat Washer - M8',
#2821,#2806);
#2814=PRODUCT_DEFINITION('Hex Nut - M8','Hex Nut - M8',#2822,
#2806);
#2815=PRODUCT_DEFINITION_FORMATION('',$,#2834);
#2816=PRODUCT_DEFINITION_FORMATION('',$,#2835);
#2817=PRODUCT_DEFINITION_FORMATION('',$,#2836);
#2818=PRODUCT_DEFINITION_FORMATION('',$,#2837);
#2819=PRODUCT_DEFINITION_FORMATION('',$,#2838);
#2820=PRODUCT_DEFINITION_FORMATION('',$,#2839);
#2821=PRODUCT_DEFINITION_FORMATION('',$,#2840);
#2822=PRODUCT_DEFINITION_FORMATION('',$,#2841);
#2823=PRODUCT_RELATED_PRODUCT_CATEGORY(
'PAT-097',
'PAT-097',(#2834));
#2824=PRODUCT_RELATED_PRODUCT_CATEGORY('Slotted grid plate',
'Slotted grid plate',(#2835));
#2825=PRODUCT_RELATED_PRODUCT_CATEGORY('M8 captive slot nut',
'M8 captive slot nut',(#2836));
#2826=PRODUCT_RELATED_PRODUCT_CATEGORY('Stepped heel block',
'Stepped heel block',(#2837));
#2827=PRODUCT_RELATED_PRODUCT_CATEGORY('Slotted clamp strap',
'Slotted clamp strap',(#2838));
#2828=PRODUCT_RELATED_PRODUCT_CATEGORY('M8 clamp stud','M8 clamp stud',
(#2839));
#2829=PRODUCT_RELATED_PRODUCT_CATEGORY('Flat Washer - M8',
'Flat Washer - M8',(#2840));
#2830=PRODUCT_RELATED_PRODUCT_CATEGORY('Hex Nut - M8','Hex Nut - M8',(#2841));
#2831=APPLICATION_PROTOCOL_DEFINITION('international standard',
'automotive_design',2009,#2832);
#2832=APPLICATION_CONTEXT(
'Core Data for Automotive Mechanical Design Process');
#2833=PRODUCT_CONTEXT('part definition',#2832,'mechanical');
#2834=PRODUCT('PAT-097',
'PAT-097',
'PAT-097',(#2833));
#2835=PRODUCT('Slotted grid plate','Slotted grid plate',
'Slotted grid plate',(#2833));
#2836=PRODUCT('M8 captive slot nut','M8 captive slot nut',
'M8 captive slot nut',(#2833));
#2837=PRODUCT('Stepped heel block','Stepped heel block',
'Stepped heel block',(#2833));
#2838=PRODUCT('Slotted clamp strap','Slotted clamp strap',
'Slotted clamp strap',(#2833));
#2839=PRODUCT('M8 clamp stud','M8 clamp stud',
'M8 clamp stud',(#2833));
#2840=PRODUCT('Flat Washer - M8','Flat Washer - M8',
'Flat Washer - M8',(#2833));
#2841=PRODUCT('Hex Nut - M8','Hex Nut - M8','Hex Nut - M8',
(#2833));
#2842=PRESENTATION_STYLE_ASSIGNMENT((#2848));
#2843=PRESENTATION_STYLE_ASSIGNMENT((#2849));
#2844=PRESENTATION_STYLE_ASSIGNMENT((#2850));
#2845=PRESENTATION_STYLE_ASSIGNMENT((#2851));
#2846=PRESENTATION_STYLE_ASSIGNMENT((#2852));
#2847=PRESENTATION_STYLE_ASSIGNMENT((#2853));
#2848=SURFACE_STYLE_USAGE(.BOTH.,#2854);
#2849=SURFACE_STYLE_USAGE(.BOTH.,#2855);
#2850=SURFACE_STYLE_USAGE(.BOTH.,#2856);
#2851=SURFACE_STYLE_USAGE(.BOTH.,#2857);
#2852=SURFACE_STYLE_USAGE(.BOTH.,#2858);
#2853=SURFACE_STYLE_USAGE(.BOTH.,#2859);
#2854=SURFACE_SIDE_STYLE('',(#2860));
#2855=SURFACE_SIDE_STYLE('',(#2861));
#2856=SURFACE_SIDE_STYLE('',(#2862));
#2857=SURFACE_SIDE_STYLE('',(#2863));
#2858=SURFACE_SIDE_STYLE('',(#2864));
#2859=SURFACE_SIDE_STYLE('',(#2865));
#2860=SURFACE_STYLE_FILL_AREA(#2866);
#2861=SURFACE_STYLE_FILL_AREA(#2867);
#2862=SURFACE_STYLE_FILL_AREA(#2868);
#2863=SURFACE_STYLE_FILL_AREA(#2869);
#2864=SURFACE_STYLE_FILL_AREA(#2870);
#2865=SURFACE_STYLE_FILL_AREA(#2871);
#2866=FILL_AREA_STYLE('Steel - Satin',(#2872));
#2867=FILL_AREA_STYLE('CAD Library Painted - Engineering blue',(#2873));
#2868=FILL_AREA_STYLE('CAD Library Painted - Light blue',(#2874));
#2869=FILL_AREA_STYLE('CAD Library Painted - Off white',(#2875));
#2870=FILL_AREA_STYLE('CAD Library Painted - Steel gray',(#2876));
#2871=FILL_AREA_STYLE('CAD Library Painted - Graphite',(#2877));
#2872=FILL_AREA_STYLE_COLOUR('Steel - Satin',#2878);
#2873=FILL_AREA_STYLE_COLOUR('CAD Library Painted - Engineering blue',#2879);
#2874=FILL_AREA_STYLE_COLOUR('CAD Library Painted - Light blue',#2880);
#2875=FILL_AREA_STYLE_COLOUR('CAD Library Painted - Off white',#2881);
#2876=FILL_AREA_STYLE_COLOUR('CAD Library Painted - Steel gray',#2882);
#2877=FILL_AREA_STYLE_COLOUR('CAD Library Painted - Graphite',#2883);
#2878=COLOUR_RGB('Steel - Satin',0.627450980392157,0.627450980392157,0.627450980392157);
#2879=COLOUR_RGB('CAD Library Painted - Engineering blue',0.12156862745098,
0.356862745098039,0.6);
#2880=COLOUR_RGB('CAD Library Painted - Light blue',0.286274509803922,0.552941176470588,
0.780392156862745);
#2881=COLOUR_RGB('CAD Library Painted - Off white',0.909803921568627,0.901960784313726,
0.858823529411765);
#2882=COLOUR_RGB('CAD Library Painted - Steel gray',0.592156862745098,0.631372549019608,
0.67843137254902);
#2883=COLOUR_RGB('CAD Library Painted - Graphite',0.0980392156862745,0.109803921568627,
0.125490196078431);
#2884=COLOUR_RGB('Dark Blue',0.08,0.2,0.34);
#2885=FILL_AREA_STYLE_COLOUR('',#2884);
#2886=FILL_AREA_STYLE('',(#2885));
#2887=SURFACE_STYLE_FILL_AREA(#2886);
#2888=SURFACE_SIDE_STYLE('',(#2887));
#2889=SURFACE_STYLE_USAGE(.BOTH.,#2888);
#2890=PRESENTATION_STYLE_ASSIGNMENT((#2889));
#2891=COLOUR_RGB('Light Blue',0.38,0.62,0.78);
#2892=FILL_AREA_STYLE_COLOUR('',#2891);
#2893=FILL_AREA_STYLE('',(#2892));
#2894=SURFACE_STYLE_FILL_AREA(#2893);
#2895=SURFACE_SIDE_STYLE('',(#2894));
#2896=SURFACE_STYLE_USAGE(.BOTH.,#2895);
#2897=PRESENTATION_STYLE_ASSIGNMENT((#2896));
#2898=COLOUR_RGB('Sky Blue',0.24,0.69,0.87);
#2899=FILL_AREA_STYLE_COLOUR('',#2898);
#2900=FILL_AREA_STYLE('',(#2899));
#2901=SURFACE_STYLE_FILL_AREA(#2900);
#2902=SURFACE_SIDE_STYLE('',(#2901));
#2903=SURFACE_STYLE_USAGE(.BOTH.,#2902);
#2904=PRESENTATION_STYLE_ASSIGNMENT((#2903));
#2905=COLOUR_RGB('Grey',0.48,0.52,0.57);
#2906=FILL_AREA_STYLE_COLOUR('',#2905);
#2907=FILL_AREA_STYLE('',(#2906));
#2908=SURFACE_STYLE_FILL_AREA(#2907);
#2909=SURFACE_SIDE_STYLE('',(#2908));
#2910=SURFACE_STYLE_USAGE(.BOTH.,#2909);
#2911=PRESENTATION_STYLE_ASSIGNMENT((#2910));
#2912=COLOUR_RGB('Black',0.12,0.14,0.17);
#2913=FILL_AREA_STYLE_COLOUR('',#2912);
#2914=FILL_AREA_STYLE('',(#2913));
#2915=SURFACE_STYLE_FILL_AREA(#2914);
#2916=SURFACE_SIDE_STYLE('',(#2915));
#2917=SURFACE_STYLE_USAGE(.BOTH.,#2916);
#2918=PRESENTATION_STYLE_ASSIGNMENT((#2917));
#2919=COLOUR_RGB('Off White',0.89,0.88,0.83);
#2920=FILL_AREA_STYLE_COLOUR('',#2919);
#2921=FILL_AREA_STYLE('',(#2920));
#2922=SURFACE_STYLE_FILL_AREA(#2921);
#2923=SURFACE_SIDE_STYLE('',(#2922));
#2924=SURFACE_STYLE_USAGE(.BOTH.,#2923);
#2925=PRESENTATION_STYLE_ASSIGNMENT((#2924));
ENDSEC;
END-ISO-10303-21;
